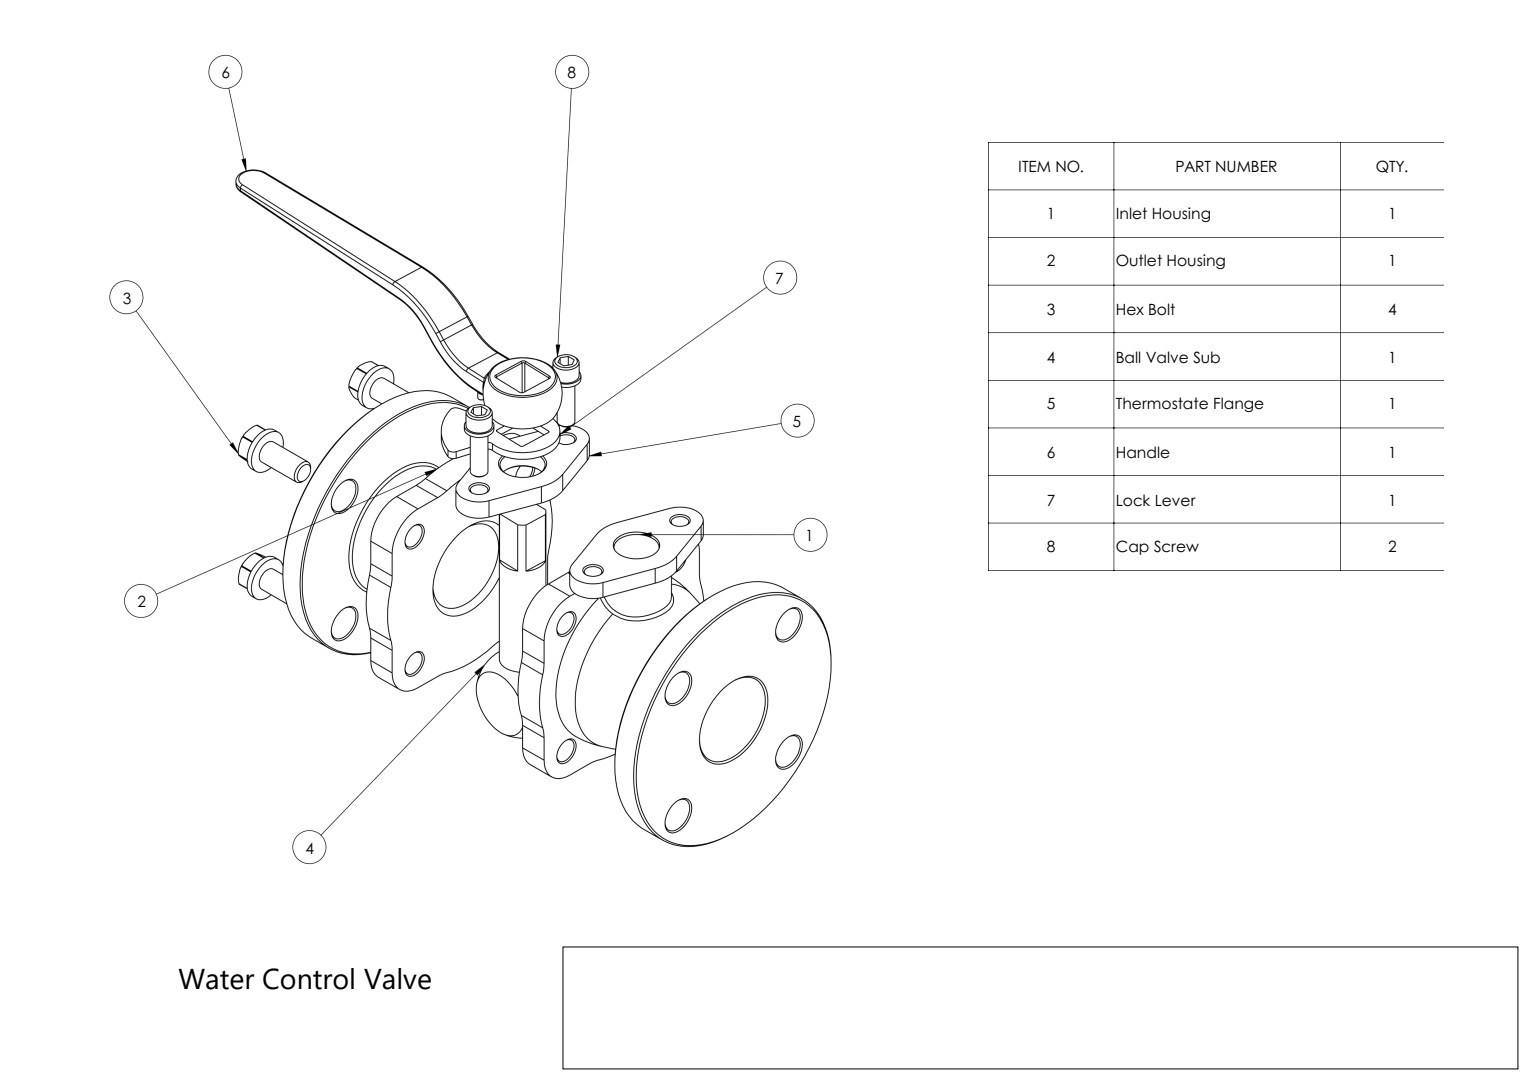
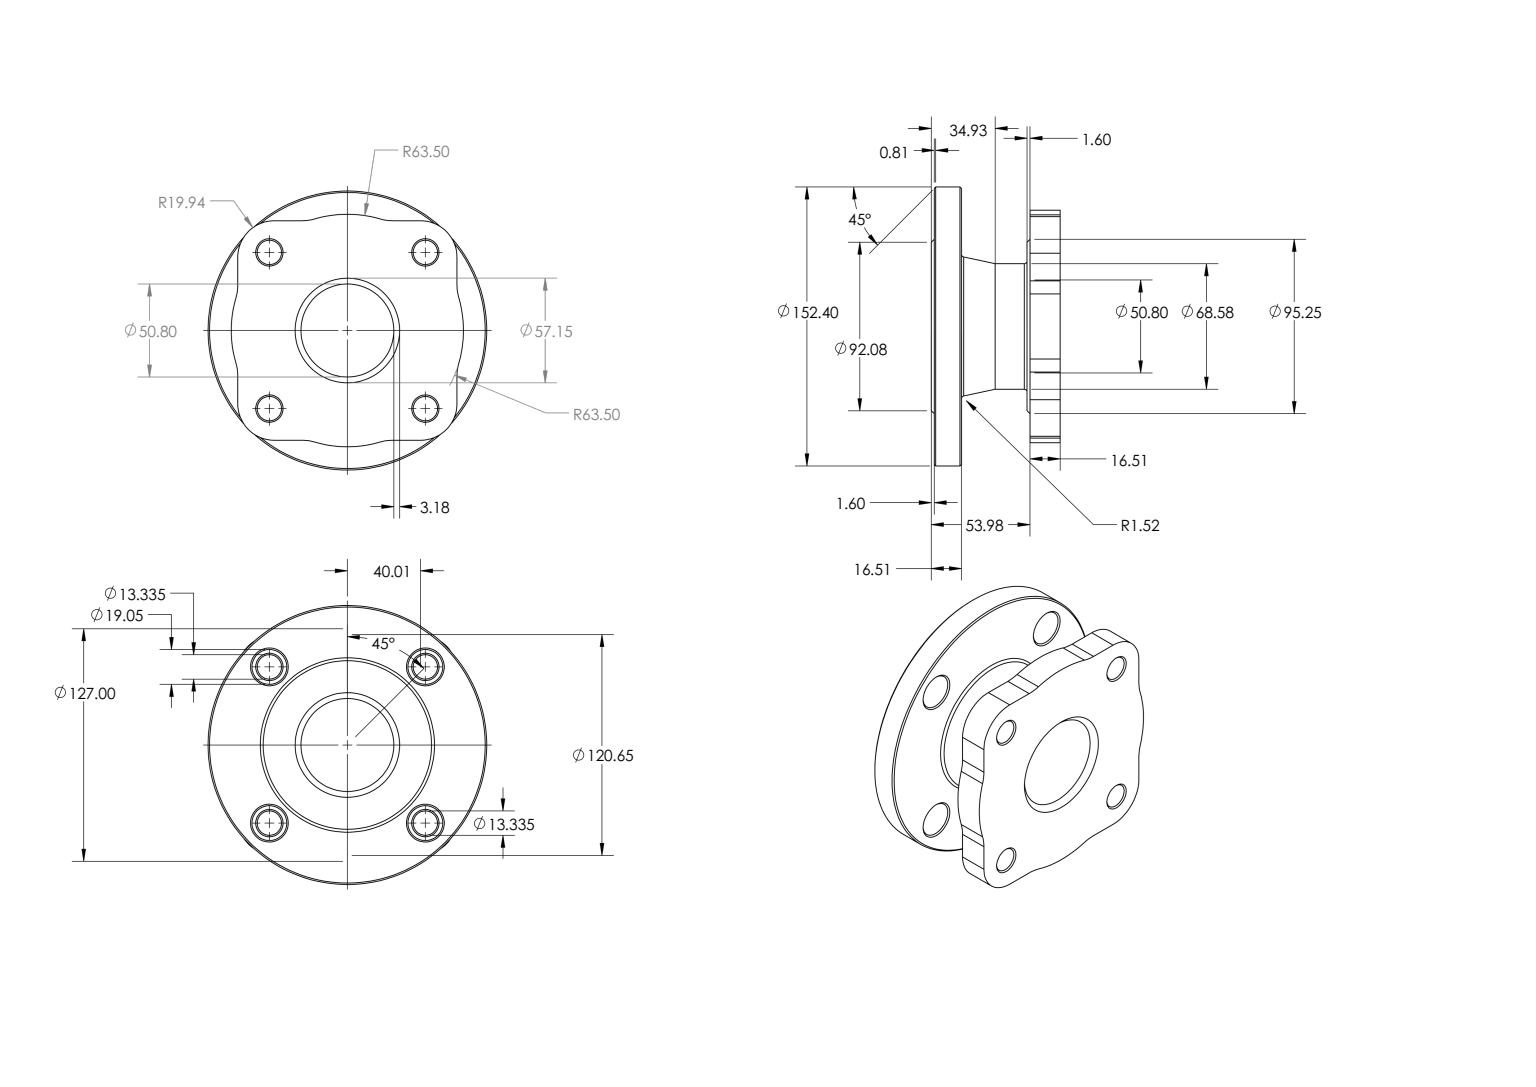
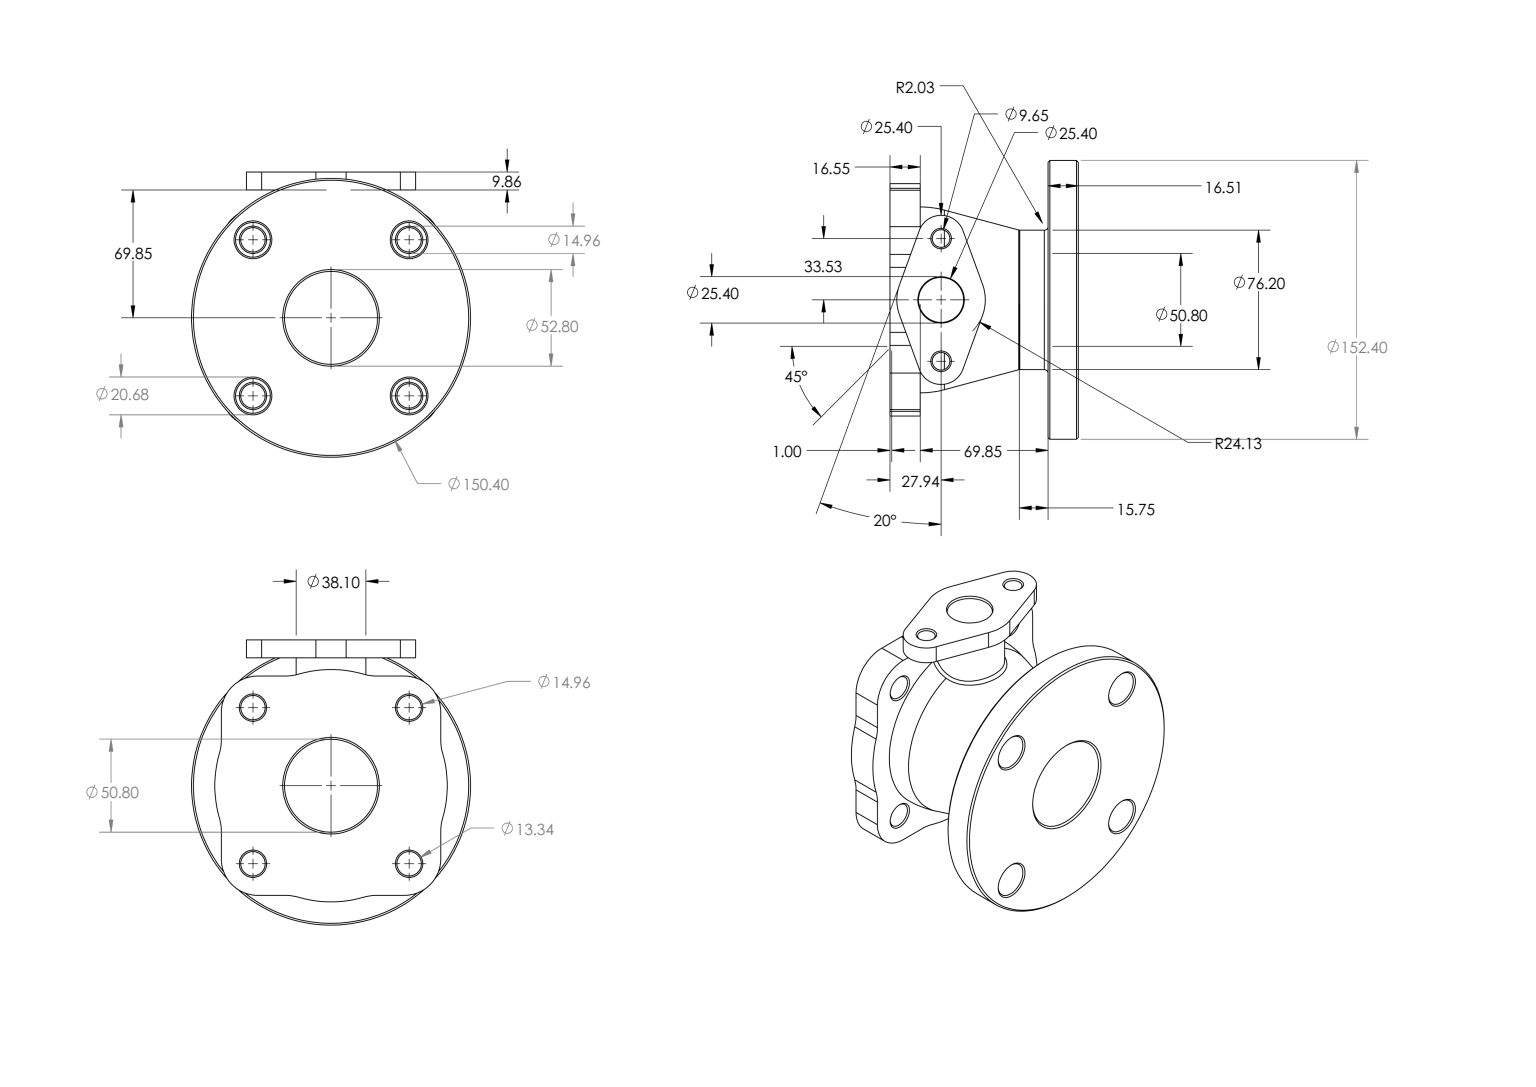
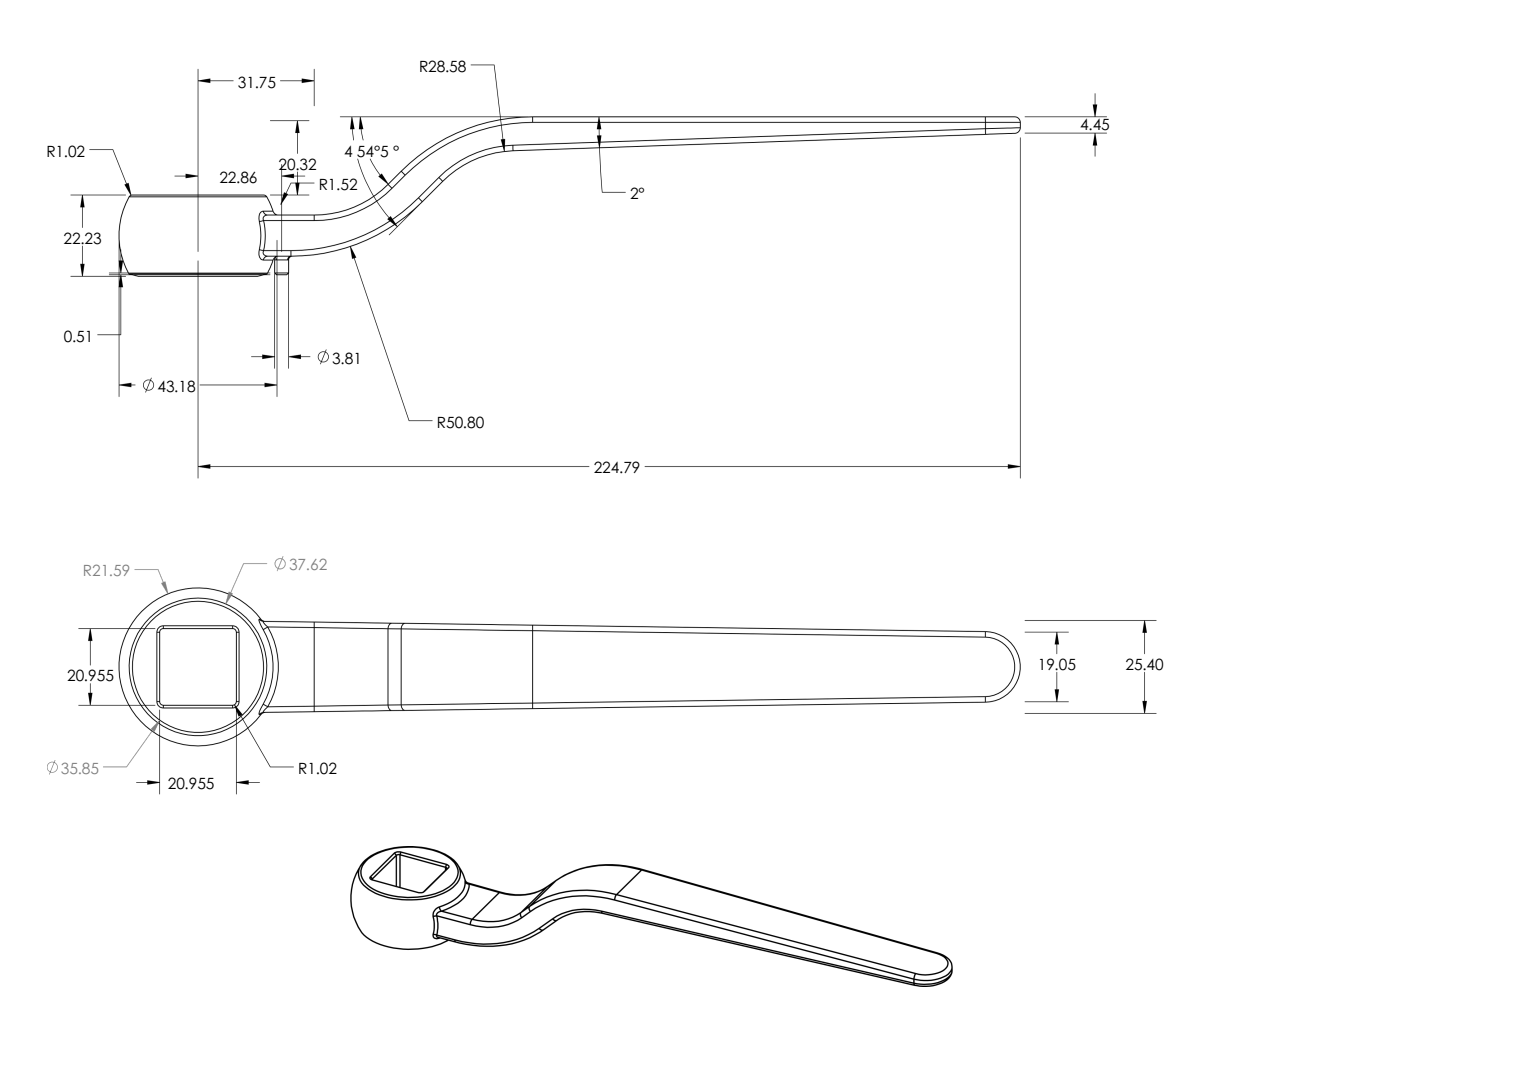
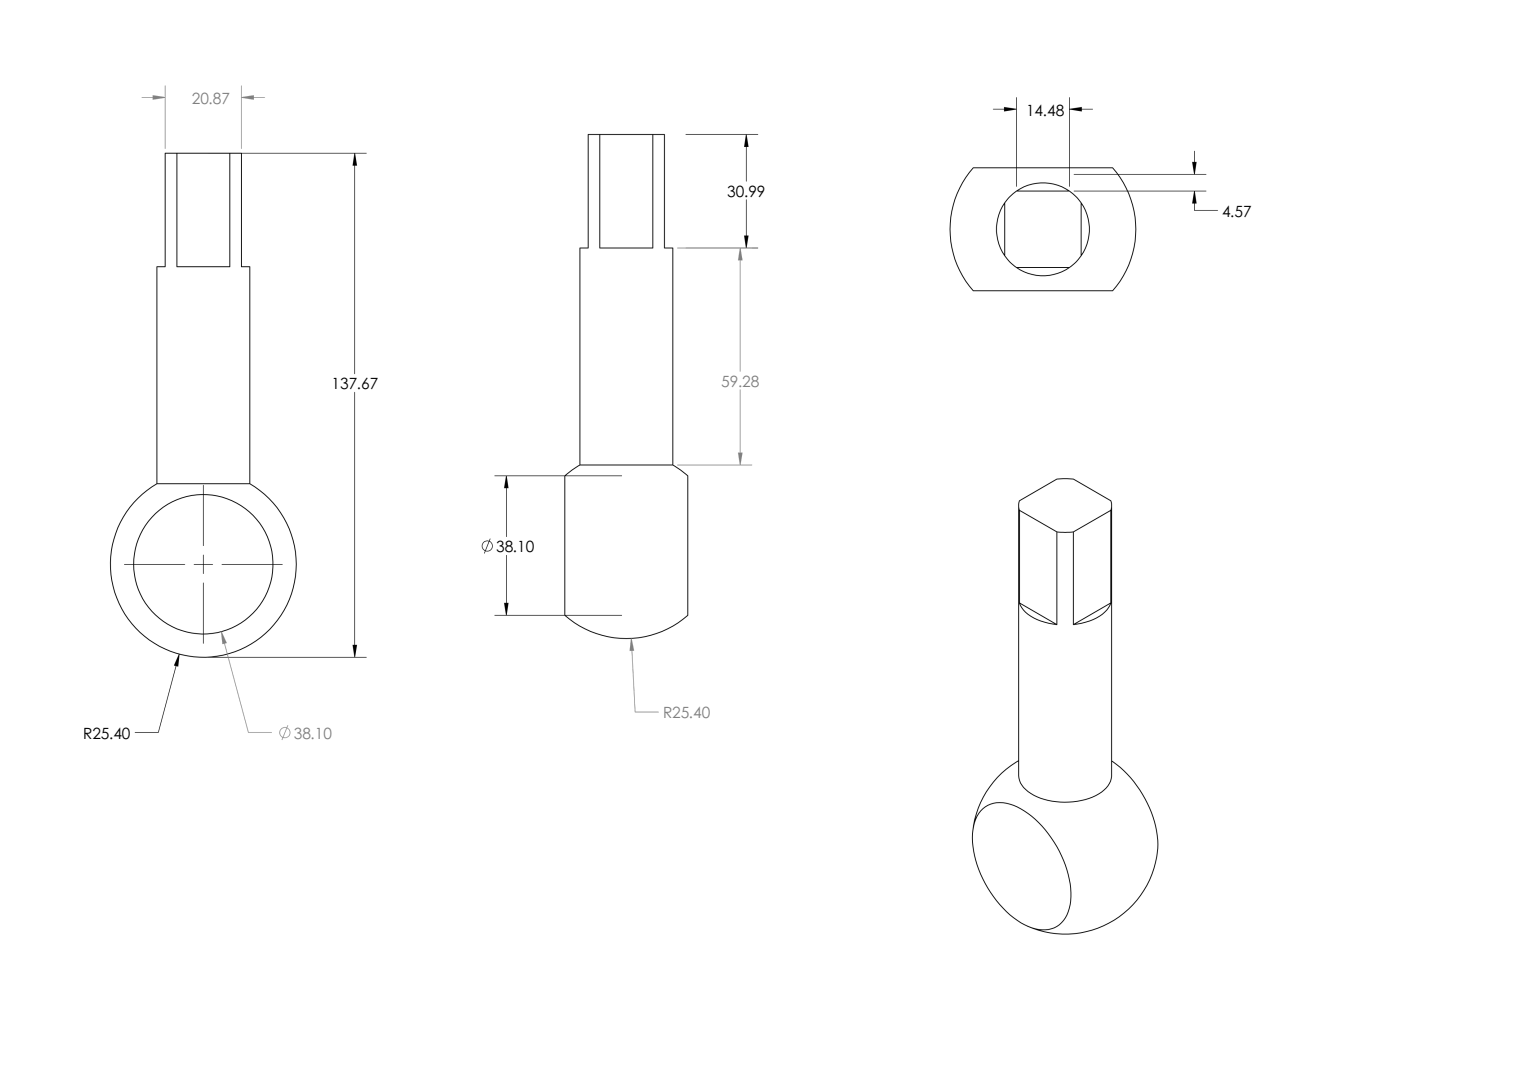
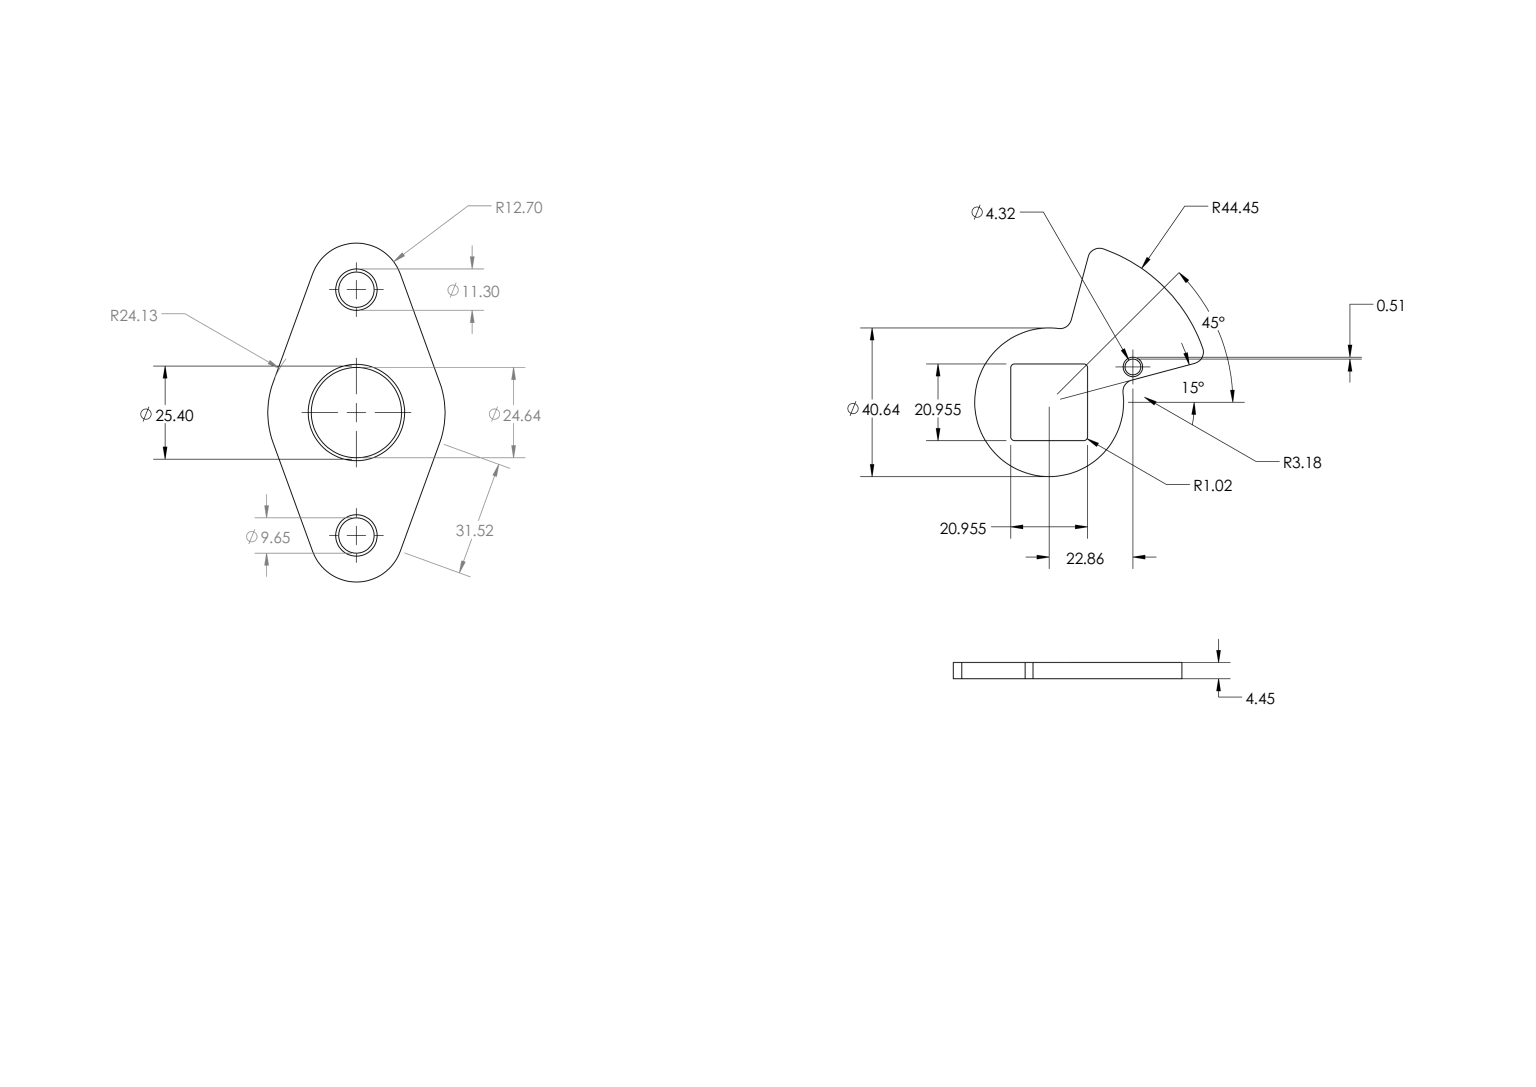
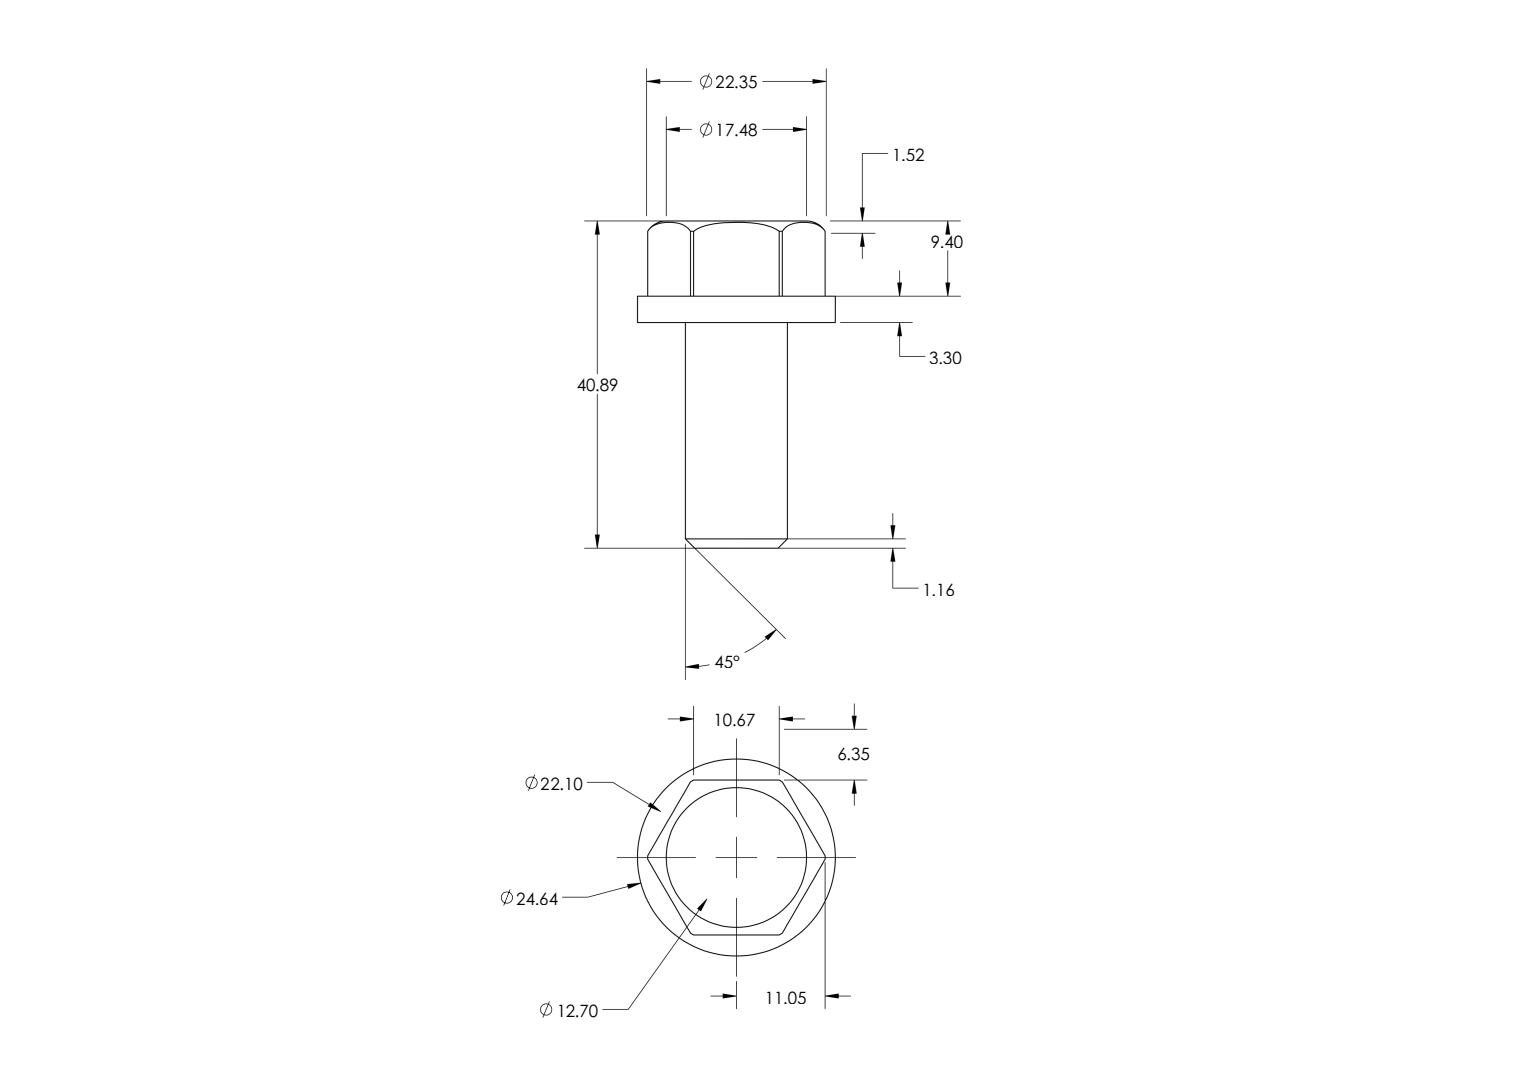
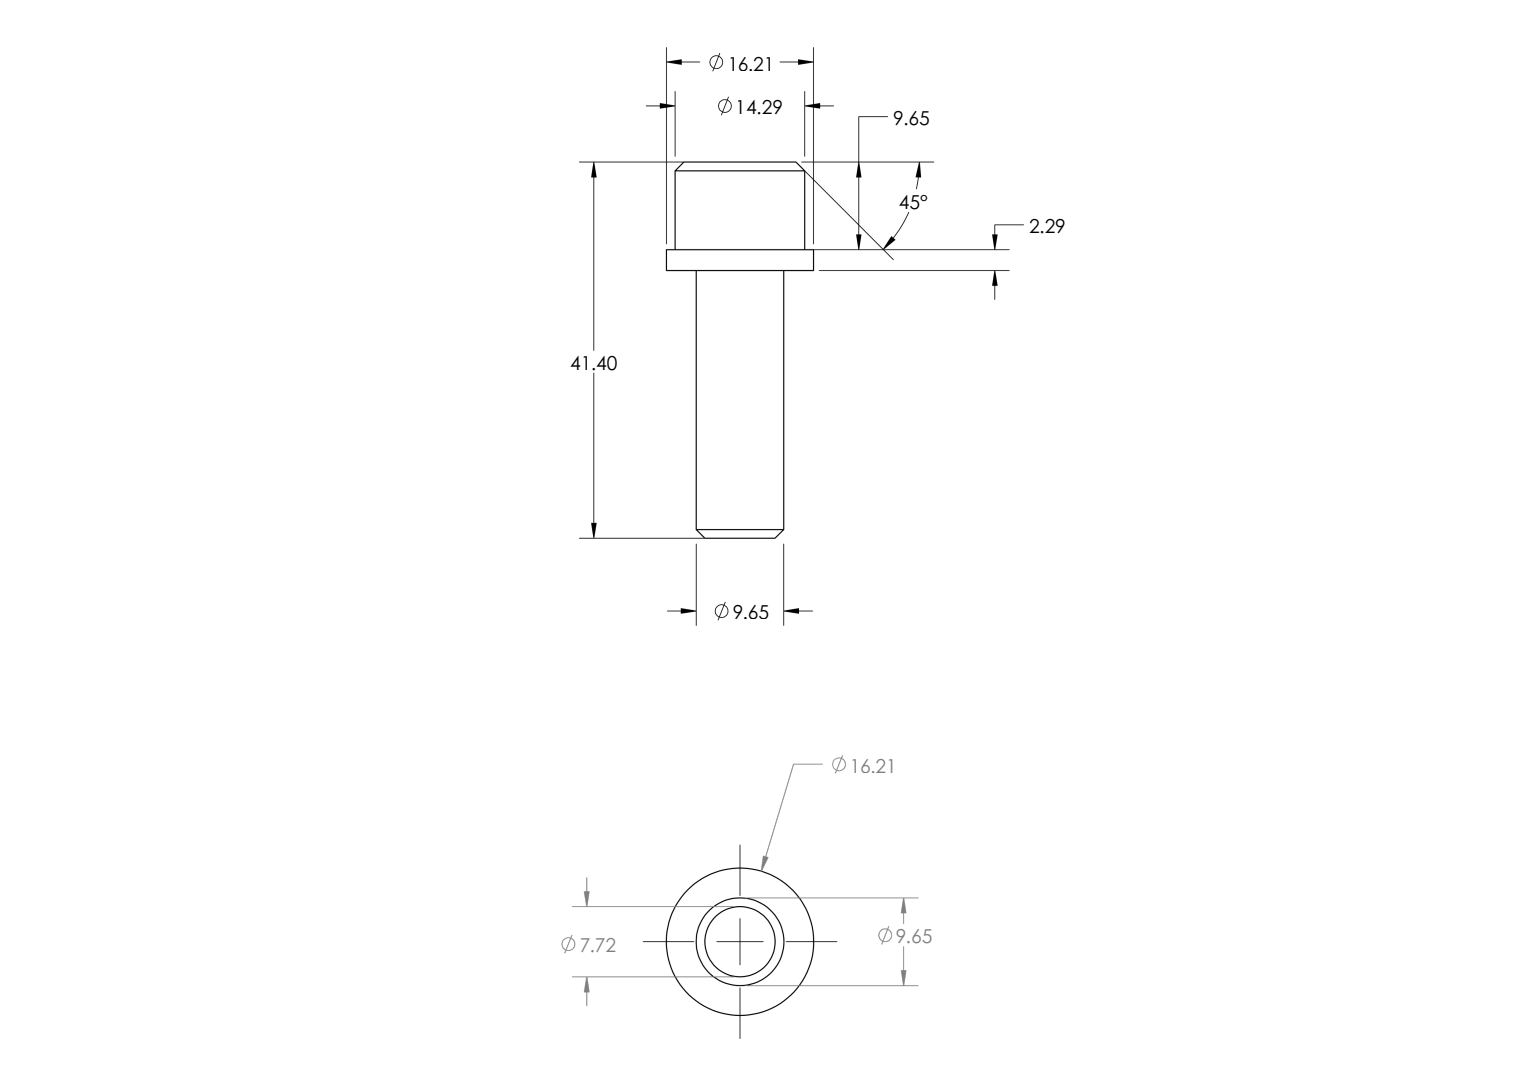
ISO-10303-21;
HEADER;
FILE_DESCRIPTION (('STEP AP214'),
    '1' );
FILE_NAME ('MAT-052',
    '2026-10-23T18:01:19',
    ( '' ),
    ( '' ),
    'SwSTEP 2.0',
    'SolidWorks 2025',
    '' );
FILE_SCHEMA (( 'AUTOMOTIVE_DESIGN' ));
ENDSEC;

DATA;
#1 = ORIENTED_EDGE ( 'NONE', *, *, #12221, .T. ) ;
#2 = CARTESIAN_POINT ( 'NONE',  ( 0.6742552310713171293, -0.4178340986603278351, 0.4797493044159374387 ) ) ;
#3 = CARTESIAN_POINT ( 'NONE',  ( 0.000000000000000000, 0.03800000000000004763, 0.000000000000000000 ) ) ;
#4 = DIRECTION ( 'NONE',  ( 0.000000000000000000, 0.000000000000000000, -1.000000000000000000 ) ) ;
#5 = ORIENTED_EDGE ( 'NONE', *, *, #15122, .F. ) ;
#6 = MECHANICAL_DESIGN_GEOMETRIC_PRESENTATION_REPRESENTATION (  '', ( #7130 ), #10291 ) ;
#7 = CYLINDRICAL_SURFACE ( 'NONE', #13072, 0.7849999999999998090 ) ;
#8 = EDGE_LOOP ( 'NONE', ( #3348, #3892, #6424, #10315, #10248, #3759, #9875, #3838 ) ) ;
#9 = DIRECTION ( 'NONE',  ( 0.000000000000000000, 1.000000000000000000, 0.000000000000000000 ) ) ;
#10 = DIRECTION ( 'NONE',  ( 0.000000000000000000, 0.000000000000000000, 1.000000000000000000 ) ) ;
#11 = ORIENTED_EDGE ( 'NONE', *, *, #1358, .T. ) ;
#12 = CARTESIAN_POINT ( 'NONE',  ( 2.742999999999999883, -1.679378605318041950, 1.679378605318059048 ) ) ;
#13 = ADVANCED_FACE ( 'NONE', ( #4673 ), #12779, .T. ) ;
#14 = CARTESIAN_POINT ( 'NONE',  ( 2.184227569363842658, 0.01449120636726281344, -0.4691493281163300333 ) ) ;
#15 = DIRECTION ( 'NONE',  ( 0.01412288512831213171, -3.675428035873182550E-19, -0.9999002670844991947 ) ) ;
#16 = AXIS2_PLACEMENT_3D ( 'NONE', #9213, #3471, #11656 ) ;
#17 = CARTESIAN_POINT ( 'NONE',  ( 2.124999999999999556, 2.359999999999994547, -1.575000000000016831 ) ) ;
#18 = CARTESIAN_POINT ( 'NONE',  ( 3.512958614626789711, 1.913572711384756708, -0.7285857137282393259 ) ) ;
#19 = ORIENTED_EDGE ( 'NONE', *, *, #5081, .F. ) ;
#20 = EDGE_LOOP ( 'NONE', ( #12977, #13926, #80, #12330, #3550, #1195, #10646, #7919 ) ) ;
#21 = CARTESIAN_POINT ( 'NONE',  ( 1.014389565038390506, -0.4429482523290907969, -0.3623444146133236177 ) ) ;
#22 = EDGE_LOOP ( 'NONE', ( #257, #9527, #1751, #1680 ) ) ;
#23 = AXIS2_PLACEMENT_3D ( 'NONE', #11429, #932, #7837 ) ;
#24 = DIRECTION ( 'NONE',  ( 0.000000000000000000, 0.000000000000000000, -1.000000000000000000 ) ) ;
#25 = CARTESIAN_POINT ( 'NONE',  ( 0.9160226681002169302, -0.4626215099191109403, -0.4483450520235250925 ) ) ;
#26 = CARTESIAN_POINT ( 'NONE',  ( 0.7513246802501661881, 0.000000000000000000, -0.4293820849162031661 ) ) ;
#27 = ORIENTED_EDGE ( 'NONE', *, *, #241, .F. ) ;
#28 = EDGE_CURVE ( 'NONE', #11196, #3954, #11572, .T. ) ;
#29 = CARTESIAN_POINT ( 'NONE',  ( 3.875000000000000000, 1.885381157978844868, -0.5000000000000002220 ) ) ;
#30 = CARTESIAN_POINT ( 'NONE',  ( 2.774999999999999911, -0.9799999999999436939, 2.360000000000016307 ) ) ;
#31 = DIRECTION ( 'NONE',  ( -1.000000000000000000, -0.000000000000000000, -0.000000000000000000 ) ) ;
#32 = CARTESIAN_POINT ( 'NONE',  ( 3.874999999999999556, 3.567999999999999616, -1.320000000000000062 ) ) ;
#33 = CARTESIAN_POINT ( 'NONE',  ( 4.627329080935005834, 1.724141250851881191, -0.2956774535502572077 ) ) ;
#34 = VERTEX_POINT ( 'NONE', #12922 ) ;
#36 = EDGE_LOOP ( 'NONE', ( #14330, #7722, #9947, #11329, #1823, #9061, #6511, #9617 ) ) ;
#35 = CARTESIAN_POINT ( 'NONE',  ( 0.4192535942842503527, 1.577705975193650412, 0.03573697939582392430 ) ) ;
#37 = ORIENTED_EDGE ( 'NONE', *, *, #11617, .T. ) ;
#38 = CARTESIAN_POINT ( 'NONE',  ( 2.774999999999999911, -2.360000000000000320, 0.9799999999999999822 ) ) ;
#39 = VERTEX_POINT ( 'NONE', #10557 ) ;
#40 = ADVANCED_FACE ( 'NONE', ( #12760 ), #3290, .F. ) ;
#41 = VECTOR ( 'NONE', #2622, 39.37007874015748143 ) ;
#42 = EDGE_CURVE ( 'NONE', #4100, #13687, #5470, .T. ) ;
#43 = DIRECTION ( 'NONE',  ( -0.9994005049267692398, -7.584452071732532247E-16, -0.03462124711963855683 ) ) ;
#44 = DIRECTION ( 'NONE',  ( 0.000000000000000000, 0.000000000000000000, -1.000000000000000000 ) ) ;
#45 = ORIENTED_EDGE ( 'NONE', *, *, #8856, .F. ) ;
#46 = EDGE_CURVE ( 'NONE', #11318, #5162, #12173, .T. ) ;
#47 = DIRECTION ( 'NONE',  ( -1.000000000000000000, -0.000000000000000000, -0.000000000000000000 ) ) ;
#48 = CARTESIAN_POINT ( 'NONE',  ( -0.09035531712817639061, 1.379999999999999671, 0.1565000000000000280 ) ) ;
#49 = DIRECTION ( 'NONE',  ( 0.000000000000000000, 0.000000000000000000, -1.000000000000000000 ) ) ;
#50 = DIRECTION ( 'NONE',  ( 0.000000000000000000, 0.000000000000000000, 1.000000000000000000 ) ) ;
#51 = AXIS2_PLACEMENT_3D ( 'NONE', #8937, #9020, #9933 ) ;
#52 = EDGE_CURVE ( 'NONE', #3395, #10754, #14120, .T. ) ;
#53 = CARTESIAN_POINT ( 'NONE',  ( 2.742999999999999883, -1.679378605318041950, 1.941878605318059003 ) ) ;
#54 = VECTOR ( 'NONE', #5461, 39.37007874015748143 ) ;
#55 = DIRECTION ( 'NONE',  ( -1.000000000000000000, -0.000000000000000000, 0.000000000000000000 ) ) ;
#56 = CARTESIAN_POINT ( 'NONE',  ( 1.375000000000000000, 1.653273178848927113E-16, -1.350000000000000089 ) ) ;
#57 = CARTESIAN_POINT ( 'NONE',  ( 0.1007315414569005807, 0.000000000000000000, -0.7936328852534507705 ) ) ;
#58 = ORIENTED_EDGE ( 'NONE', *, *, #5402, .F. ) ;
#59 = AXIS2_PLACEMENT_3D ( 'NONE', #1494, #12413, #11192 ) ;
#60 = CARTESIAN_POINT ( 'NONE',  ( 3.426491571325181340, -1.679378605318059048, -1.679378605318041950 ) ) ;
#62 = ORIENTED_EDGE ( 'NONE', *, *, #9280, .T. ) ;
#61 = PLANE ( 'NONE',  #8465 ) ;
#63 = ORIENTED_EDGE ( 'NONE', *, *, #4346, .F. ) ;
#64 = CARTESIAN_POINT ( 'NONE',  ( 3.601417382415921686, 1.056999999999999718, -0.3891265382754440227 ) ) ;
#65 = DIRECTION ( 'NONE',  ( 0.000000000000000000, 0.000000000000000000, 1.000000000000000000 ) ) ;
#66 = ORIENTED_EDGE ( 'NONE', *, *, #9058, .F. ) ;
#67 = FACE_OUTER_BOUND ( 'NONE', #2223, .T. ) ;
#68 = CARTESIAN_POINT ( 'NONE',  ( 0.6601485485260571995, -0.3723516483516483011, -0.5137583810202324131 ) ) ;
#69 = AXIS2_PLACEMENT_3D ( 'NONE', #6911, #5755, #13762 ) ;
#70 = CARTESIAN_POINT ( 'NONE',  ( 0.9652173913043479159, -0.4829999999999998739, -0.3379636412230419551 ) ) ;
#71 = ADVANCED_FACE ( 'NONE', ( #976 ), #2655, .T. ) ;
#72 = ORIENTED_EDGE ( 'NONE', *, *, #13429, .F. ) ;
#73 = DIRECTION ( 'NONE',  ( 0.000000000000000000, 0.000000000000000000, 1.000000000000000000 ) ) ;
#74 = CARTESIAN_POINT ( 'NONE',  ( 0.6773748815706875925, -0.3764079396444214298, 0.4904325581699060521 ) ) ;
#75 = CARTESIAN_POINT ( 'NONE',  ( 2.774999999999999911, 1.679378605318042395, -1.679378605318058604 ) ) ;
#76 = DIRECTION ( 'NONE',  ( 0.3420201433256623846, 0.000000000000000000, 0.9396926207859106484 ) ) ;
#77 = ORIENTED_EDGE ( 'NONE', *, *, #5878, .F. ) ;
#78 = EDGE_CURVE ( 'NONE', #7551, #8303, #4616, .T. ) ;
#79 = FACE_OUTER_BOUND ( 'NONE', #9861, .T. ) ;
#80 = ORIENTED_EDGE ( 'NONE', *, *, #10085, .T. ) ;
#81 = DIRECTION ( 'NONE',  ( 0.000000000000000000, 0.000000000000000000, -1.000000000000000000 ) ) ;
#82 = ORIENTED_EDGE ( 'NONE', *, *, #11617, .F. ) ;
#83 = AXIS2_PLACEMENT_3D ( 'NONE', #10254, #9341, #11313 ) ;
#84 = DIRECTION ( 'NONE',  ( -0.000000000000000000, -1.000000000000000000, -0.000000000000000000 ) ) ;
#85 = FACE_OUTER_BOUND ( 'NONE', #9329, .T. ) ;
#86 = DIRECTION ( 'NONE',  ( 0.000000000000000000, 0.000000000000000000, 1.000000000000000000 ) ) ;
#87 = DIRECTION ( 'NONE',  ( -1.000000000000000000, -0.000000000000000000, -0.000000000000000000 ) ) ;
#88 = EDGE_CURVE ( 'NONE', #13385, #4765, #4744, .T. ) ;
#89 = EDGE_LOOP ( 'NONE', ( #7077, #10683, #6520, #11153 ) ) ;
#90 = ORIENTED_EDGE ( 'NONE', *, *, #12016, .T. ) ;
#91 = ORIENTED_EDGE ( 'NONE', *, *, #3376, .F. ) ;
#92 = FACE_BOUND ( 'NONE', #13262, .T. ) ;
#93 = DIRECTION ( 'NONE',  ( -0.000000000000000000, -1.000000000000000000, -0.000000000000000000 ) ) ;
#94 = LINE ( 'NONE', #8250, #10804 ) ;
#95 = CARTESIAN_POINT ( 'NONE',  ( 0.000000000000000000, 4.529999999999999361, 0.000000000000000000 ) ) ;
#96 = AXIS2_PLACEMENT_3D ( 'NONE', #10060, #3097, #1937 ) ;
#97 = CARTESIAN_POINT ( 'NONE',  ( 0.7020471549603389816, -0.02897145875702579823, -0.4816513823572634578 ) ) ;
#98 = ORIENTED_EDGE ( 'NONE', *, *, #14017, .F. ) ;
#99 = CARTESIAN_POINT ( 'NONE',  ( 0.4125000000000000333, 0.1749999999999999889, 0.3724999999999999978 ) ) ;
#100 = AXIS2_PLACEMENT_3D ( 'NONE', #9537, #4707, #14178 ) ;
#101 = AXIS2_PLACEMENT_3D ( 'NONE', #4920, #3459, #11799 ) ;
#102 = DIRECTION ( 'NONE',  ( 0.000000000000000000, 1.000000000000000000, -0.000000000000000000 ) ) ;
#103 = CARTESIAN_POINT ( 'NONE',  ( 3.390179639970223313, 0.6913388717410868800, -0.3921396980529558429 ) ) ;
#104 = FACE_OUTER_BOUND ( 'NONE', #11519, .T. ) ;
#105 = VECTOR ( 'NONE', #3673, 39.37007874015748854 ) ;
#106 = CARTESIAN_POINT ( 'NONE',  ( 4.657203315104130326, 1.728603760376735909, 0.2078873897356731115 ) ) ;
#107 = ORIENTED_EDGE ( 'NONE', *, *, #12678, .F. ) ;
#108 = CIRCLE ( 'NONE', #2074, 0.03999999999999998002 ) ;
#110 = ORIENTED_EDGE ( 'NONE', *, *, #10895, .T. ) ;
#109 = DIRECTION ( 'NONE',  ( 0.000000000000000000, 0.000000000000000000, -1.000000000000000000 ) ) ;
#111 = CIRCLE ( 'NONE', #4039, 0.3750000000000004996 ) ;
#112 = ORIENTED_EDGE ( 'NONE', *, *, #14877, .T. ) ;
#113 = CARTESIAN_POINT ( 'NONE',  ( 0.8418300605894719624, -0.4829999999999998739, -0.3276580719765713745 ) ) ;
#114 = VERTEX_POINT ( 'NONE', #12839 ) ;
#115 = CARTESIAN_POINT ( 'NONE',  ( 6.826491571325181695, 0.000000000000000000, 0.000000000000000000 ) ) ;
#116 = APPLICATION_PROTOCOL_DEFINITION ( 'draft international standard', 'automotive_design', 1998, #8901 ) ;
#117 = CARTESIAN_POINT ( 'NONE',  ( 2.774999999999999911, 3.360000000000016751, 0.9799999999999461364 ) ) ;
#118 = ORIENTED_EDGE ( 'NONE', *, *, #160, .F. ) ;
#119 = CARTESIAN_POINT ( 'NONE',  ( -0.09057123220595257596, 1.599173898159329976, -0.3809527529760086129 ) ) ;
#120 = CARTESIAN_POINT ( 'NONE',  ( 2.061999999999999389, 0.000000000000000000, 0.000000000000000000 ) ) ;
#121 = CIRCLE ( 'NONE', #850, 0.1899999999999996136 ) ;
#122 = CARTESIAN_POINT ( 'NONE',  ( 3.874999999999999556, 2.750000000000000000, -1.320000000000000062 ) ) ;
#123 = CIRCLE ( 'NONE', #13312, 0.2944999999999987073 ) ;
#124 = CIRCLE ( 'NONE', #8691, 0.9999999999999996669 ) ;
#125 = ADVANCED_FACE ( 'NONE', ( #8119 ), #11202, .T. ) ;
#126 = DIRECTION ( 'NONE',  ( 0.000000000000000000, 0.000000000000000000, 1.000000000000000000 ) ) ;
#127 = CARTESIAN_POINT ( 'NONE',  ( 2.124999999999999556, -0.6999999999999598765, 2.400000000000012346 ) ) ;
#128 = DIRECTION ( 'NONE',  ( 0.7071067811865459074, -0.7071067811865492381, 0.000000000000000000 ) ) ;
#129 = AXIS2_PLACEMENT_3D ( 'NONE', #12929, #1218, #11933 ) ;
#130 = ORIENTED_EDGE ( 'NONE', *, *, #6487, .T. ) ;
#131 = CARTESIAN_POINT ( 'NONE',  ( 2.774999999999999911, 2.360000000000015863, 1.574999999999999956 ) ) ;
#133 = EDGE_LOOP ( 'NONE', ( #9480, #11934, #9524, #6761 ) ) ;
#132 = CARTESIAN_POINT ( 'NONE',  ( 0.000000000000000000, 0.000000000000000000, 0.000000000000000000 ) ) ;
#134 = ORIENTED_EDGE ( 'NONE', *, *, #1959, .F. ) ;
#135 = CIRCLE ( 'NONE', #14993, 0.7849999999999993650 ) ;
#136 = FACE_OUTER_BOUND ( 'NONE', #12337, .T. ) ;
#137 = ADVANCED_FACE ( 'NONE', ( #6971 ), #13149, .T. ) ;
#138 = CARTESIAN_POINT ( 'NONE',  ( 0.2849999999999996425, 0.000000000000000000, 0.4108223460329292753 ) ) ;
#139 = LINE ( 'NONE', #8292, #12561 ) ;
#140 = EDGE_LOOP ( 'NONE', ( #8999, #12949, #3584, #329, #10455, #10394, #1093, #10887, #312, #1729, #3941 ) ) ;
#141 = CARTESIAN_POINT ( 'NONE',  ( 2.124999999999999556, -1.679378605318041950, 1.973878605318058810 ) ) ;
#142 = CIRCLE ( 'NONE', #9202, 0.3750000000000007772 ) ;
#143 = PLANE ( 'NONE',  #5754 ) ;
#144 = EDGE_CURVE ( 'NONE', #5162, #1223, #2289, .T. ) ;
#145 = CARTESIAN_POINT ( 'NONE',  ( 6.123233995736763571E-17, 4.529999999999999361, 0.4999999999999997224 ) ) ;
#146 = ORIENTED_EDGE ( 'NONE', *, *, #13885, .T. ) ;
#147 = EDGE_CURVE ( 'NONE', #7267, #14527, #433, .T. ) ;
#148 = CARTESIAN_POINT ( 'NONE',  ( 0.6894183887957248125, -0.4431162156558585696, 0.4464953827605262493 ) ) ;
#149 = CONICAL_SURFACE ( 'NONE', #9948, 0.2944999999999987073, 0.7853981633974366217 ) ;
#150 = CARTESIAN_POINT ( 'NONE',  ( 3.875000000000000000, 3.137999999999999901, 0.5000000000000002220 ) ) ;
#151 = DIRECTION ( 'NONE',  ( -1.000000000000000000, -0.000000000000000000, -0.000000000000000000 ) ) ;
#152 = EDGE_LOOP ( 'NONE', ( #2875, #13382, #6419, #11719 ) ) ;
#153 = CYLINDRICAL_SURFACE ( 'NONE', #7144, 1.000000000000000444 ) ;
#154 = CARTESIAN_POINT ( 'NONE',  ( -0.4349147617188414694, 0.7512260236060024354, -0.008611041693271251005 ) ) ;
#155 = ORIENTED_EDGE ( 'NONE', *, *, #13397, .T. ) ;
#156 = EDGE_CURVE ( 'NONE', #504, #12467, #11937, .T. ) ;
#157 = CIRCLE ( 'NONE', #12372, 0.05999999999999990757 ) ;
#158 = DIRECTION ( 'NONE',  ( 1.000000000000000000, 0.000000000000000000, 0.000000000000000000 ) ) ;
#159 = VERTEX_POINT ( 'NONE', #11630 ) ;
#160 = EDGE_CURVE ( 'NONE', #1104, #11415, #8533, .T. ) ;
#161 = CARTESIAN_POINT ( 'NONE',  ( 3.426491571325181340, -1.679378605318041950, 1.384878605318060174 ) ) ;
#162 = FACE_OUTER_BOUND ( 'NONE', #5866, .T. ) ;
#163 = TOROIDAL_SURFACE ( 'NONE', #642, 0.3203340137431718859, 0.05999999999999999778 ) ;
#164 = CARTESIAN_POINT ( 'NONE',  ( -0.3724999999999999423, 0.1749999999999999889, 0.3724999999999999978 ) ) ;
#165 = CARTESIAN_POINT ( 'NONE',  ( 3.874999999999999556, 3.567999999999999616, -1.320000000000000062 ) ) ;
#166 = ORIENTED_EDGE ( 'NONE', *, *, #13997, .F. ) ;
#167 = VERTEX_POINT ( 'NONE', #2214 ) ;
#168 = DIRECTION ( 'NONE',  ( 1.000000000000000000, 0.000000000000000000, 0.000000000000000000 ) ) ;
#169 = AXIS2_PLACEMENT_3D ( 'NONE', #3610, #8290, #3527 ) ;
#170 = EDGE_LOOP ( 'NONE', ( #1546, #1638, #4736, #4813 ) ) ;
#171 = EDGE_CURVE ( 'NONE', #13385, #5675, #9017, .T. ) ;
#172 = DIRECTION ( 'NONE',  ( 1.000000000000000000, 0.000000000000000000, 0.000000000000000000 ) ) ;
#173 = CARTESIAN_POINT ( 'NONE',  ( -0.3725000000000000533, -0.6590000000000000302, 0.3724999999999999423 ) ) ;
#174 = EDGE_CURVE ( 'NONE', #282, #4996, #14362, .T. ) ;
#175 = CARTESIAN_POINT ( 'NONE',  ( 0.8848438321385330152, -0.4627371489994540066, -0.4487466038575088079 ) ) ;
#176 = DIRECTION ( 'NONE',  ( 0.01412288512831128343, 0.000000000000000000, 0.9999002670844990837 ) ) ;
#177 = ORIENTED_EDGE ( 'NONE', *, *, #5280, .F. ) ;
#178 = CARTESIAN_POINT ( 'NONE',  ( 3.652559170054249904, 1.936257245559476869, -0.4479448007622380823 ) ) ;
#179 = CONICAL_SURFACE ( 'NONE', #7293, 0.5174999999999995159, 0.7853981633974514986 ) ;
#180 = ADVANCED_FACE ( 'NONE', ( #3680 ), #7071, .F. ) ;
#181 = CARTESIAN_POINT ( 'NONE',  ( 1.397260334976607732, 0.007251848866960360247, 0.4201477693899102750 ) ) ;
#182 = DIRECTION ( 'NONE',  ( 0.000000000000000000, 0.000000000000000000, -1.000000000000000000 ) ) ;
#183 = VECTOR ( 'NONE', #7595, 39.37007874015748143 ) ;
#184 = VERTEX_POINT ( 'NONE', #11856 ) ;
#186 = EDGE_LOOP ( 'NONE', ( #11801, #8509, #1158, #8869 ) ) ;
#185 = CARTESIAN_POINT ( 'NONE',  ( 2.774999999999999911, 0.000000000000000000, 0.000000000000000000 ) ) ;
#187 = ORIENTED_EDGE ( 'NONE', *, *, #8888, .T. ) ;
#188 = DIRECTION ( 'NONE',  ( 1.000000000000000000, 0.000000000000000000, 0.000000000000000000 ) ) ;
#189 = ORIENTED_EDGE ( 'NONE', *, *, #6062, .T. ) ;
#190 = CARTESIAN_POINT ( 'NONE',  ( 3.426491571325181340, 0.000000000000000000, 0.000000000000000000 ) ) ;
#191 = ITEM_DEFINED_TRANSFORMATION ( 'NONE', 'NONE', #14264,  #8424 ) ;
#192 = FACE_BOUND ( 'NONE', #6135, .T. ) ;
#193 = VERTEX_POINT ( 'NONE', #1581 ) ;
#194 = CIRCLE ( 'NONE', #13862, 0.4349999999999999978 ) ;
#195 = CARTESIAN_POINT ( 'NONE',  ( -0.1702285915635917690, 1.581112972951822293, -0.3809527529760087239 ) ) ;
#196 = PLANE ( 'NONE',  #6331 ) ;
#197 = AXIS2_PLACEMENT_3D ( 'NONE', #7203, #5970, #10632 ) ;
#198 = EDGE_CURVE ( 'NONE', #9755, #1223, #6326, .T. ) ;
#199 = FACE_OUTER_BOUND ( 'NONE', #10241, .T. ) ;
#200 = DIRECTION ( 'NONE',  ( -1.000000000000000000, 0.000000000000000000, -1.047444401652940007E-14 ) ) ;
#201 = AXIS2_PLACEMENT_3D ( 'NONE', #268, #9637, #13052 ) ;
#202 = AXIS2_PLACEMENT_3D ( 'NONE', #13035, #253, #10606 ) ;
#203 = PLANE ( 'NONE',  #5048 ) ;
#204 = CARTESIAN_POINT ( 'NONE',  ( 0.4193347797797013499, 0.1749999999999999889, -1.564978703518711711 ) ) ;
#205 = LINE ( 'NONE', #13137, #4871 ) ;
#206 = CARTESIAN_POINT ( 'NONE',  ( 4.545987629778766248, 1.714706108888804481, 0.4425078797212881887 ) ) ;
#207 = ORIENTED_EDGE ( 'NONE', *, *, #6693, .F. ) ;
#208 = AXIS2_PLACEMENT_3D ( 'NONE', #5410, #13799, #3334 ) ;
#209 = DIRECTION ( 'NONE',  ( 0.000000000000000000, 0.000000000000000000, 1.000000000000000000 ) ) ;
#211 = ORIENTED_EDGE ( 'NONE', *, *, #10111, .F. ) ;
#210 = DIRECTION ( 'NONE',  ( -1.000000000000000000, -0.000000000000000000, -0.000000000000000000 ) ) ;
#212 = ORIENTED_EDGE ( 'NONE', *, *, #11674, .T. ) ;
#213 = VECTOR ( 'NONE', #1409, 39.37007874015748143 ) ;
#214 = FACE_OUTER_BOUND ( 'NONE', #11433, .T. ) ;
#215 = LENGTH_MEASURE_WITH_UNIT ( LENGTH_MEASURE( 0.02539999999999999897 ), #6283 );
#216 = DIRECTION ( 'NONE',  ( 1.000000000000000000, 0.000000000000000000, 0.000000000000000000 ) ) ;
#217 = ORIENTED_EDGE ( 'NONE', *, *, #5293, .F. ) ;
#218 = CARTESIAN_POINT ( 'NONE',  ( 6.787121492585022509, 0.000000000000000000, 0.000000000000000000 ) ) ;
#219 = ADVANCED_FACE ( 'NONE', ( #3751 ), #1356, .F. ) ;
#220 = CARTESIAN_POINT ( 'NONE',  ( 3.601417382415921686, 1.056999999999999718, 0.5000000000000000000 ) ) ;
#221 = DIRECTION ( 'NONE',  ( 0.01412288512831213171, -3.675428035873182550E-19, 0.9999002670844991947 ) ) ;
#222 = AXIS2_PLACEMENT_3D ( 'NONE', #2084, #6691, #5471 ) ;
#223 = ORIENTED_EDGE ( 'NONE', *, *, #6094, .T. ) ;
#224 = CARTESIAN_POINT ( 'NONE',  ( 0.4425000000000003375, 0.2159999999999999420, 0.3724999999999999423 ) ) ;
#225 = LINE ( 'NONE', #9876, #6827 ) ;
#226 = PLANE ( 'NONE',  #3739 ) ;
#227 = CARTESIAN_POINT ( 'NONE',  ( 0.7936328852534488831, 0.1749999999999999889, -0.1007315414569159018 ) ) ;
#228 = ORIENTED_EDGE ( 'NONE', *, *, #3551, .T. ) ;
#229 = DIRECTION ( 'NONE',  ( 0.7071067811865474617, 8.659560562354932858E-17, 0.7071067811865474617 ) ) ;
#230 = ORIENTED_EDGE ( 'NONE', *, *, #13541, .F. ) ;
#231 = CARTESIAN_POINT ( 'NONE',  ( -0.2846118995245673911, 1.599166939805956256, 0.2689432355367775695 ) ) ;
#232 = ORIENTED_EDGE ( 'NONE', *, *, #13602, .F. ) ;
#233 = EDGE_CURVE ( 'NONE', #5394, #8971, #13378, .T. ) ;
#234 = CARTESIAN_POINT ( 'NONE',  ( 3.874999999999999556, 3.567999999999999616, -1.130000000000000560 ) ) ;
#235 = EDGE_CURVE ( 'NONE', #5730, #4833, #8634, .T. ) ;
#236 = EDGE_CURVE ( 'NONE', #4318, #1348, #8143, .T. ) ;
#237 = LINE ( 'NONE', #14244, #10985 ) ;
#238 = CARTESIAN_POINT ( 'NONE',  ( 1.000847373107697891, -0.4430000000000000049, 0.4858637376679703634 ) ) ;
#239 = FACE_OUTER_BOUND ( 'NONE', #14821, .T. ) ;
#240 = DIRECTION ( 'NONE',  ( -0.000000000000000000, 1.000000000000000000, -0.000000000000000000 ) ) ;
#241 = EDGE_CURVE ( 'NONE', #287, #6694, #6272, .T. ) ;
#242 = LINE ( 'NONE', #7239, #4272 ) ;
#243 = AXIS2_PLACEMENT_3D ( 'NONE', #9319, #1107, #15044 ) ;
#244 = ORIENTED_EDGE ( 'NONE', *, *, #5155, .F. ) ;
#245 = ORIENTED_EDGE ( 'NONE', *, *, #2104, .F. ) ;
#246 = ORIENTED_EDGE ( 'NONE', *, *, #3419, .T. ) ;
#247 = CARTESIAN_POINT ( 'NONE',  ( 1.012992808803494293, -0.4429593110677563228, -0.3529645107950314387 ) ) ;
#248 = FACE_OUTER_BOUND ( 'NONE', #14126, .T. ) ;
#249 = CARTESIAN_POINT ( 'NONE',  ( 3.602264755523620465, 0.9969999999999996643, 0.4491205543005138412 ) ) ;
#250 = DIRECTION ( 'NONE',  ( 0.000000000000000000, 1.000000000000000000, -0.000000000000000000 ) ) ;
#251 = VERTEX_POINT ( 'NONE', #2745 ) ;
#252 = DIRECTION ( 'NONE',  ( -1.150251786806006500E-15, 0.000000000000000000, 1.000000000000000000 ) ) ;
#253 = DIRECTION ( 'NONE',  ( 1.365923996832131609E-16, -1.000000000000000000, -0.000000000000000000 ) ) ;
#254 = CYLINDRICAL_SURFACE ( 'NONE', #1961, 2.500000000000000444 ) ;
#255 = EDGE_CURVE ( 'NONE', #14724, #7714, #12509, .T. ) ;
#256 = CIRCLE ( 'NONE', #12476, 0.4999999999999995004 ) ;
#257 = ORIENTED_EDGE ( 'NONE', *, *, #5350, .T. ) ;
#259 = VERTEX_POINT ( 'NONE', #10708 ) ;
#258 = DIRECTION ( 'NONE',  ( -1.000000000000000000, -0.000000000000000000, -0.000000000000000000 ) ) ;
#260 = EDGE_CURVE ( 'NONE', #10245, #11406, #12148, .T. ) ;
#261 = VERTEX_POINT ( 'NONE', #9572 ) ;
#262 = CARTESIAN_POINT ( 'NONE',  ( 0.7058998964907862161, -0.05999999999999994227, -0.4900296624789436950 ) ) ;
#263 = ORIENTED_EDGE ( 'NONE', *, *, #11976, .T. ) ;
#264 = APPLICATION_PROTOCOL_DEFINITION ( 'draft international standard', 'automotive_design', 1998, #1849 ) ;
#265 = CARTESIAN_POINT ( 'NONE',  ( 0.6601485485260571995, -0.07064835164835162051, 0.5137583810202324131 ) ) ;
#266 = ORIENTED_EDGE ( 'NONE', *, *, #8038, .T. ) ;
#267 = DIRECTION ( 'NONE',  ( 0.000000000000000000, 0.000000000000000000, -1.000000000000000000 ) ) ;
#268 = CARTESIAN_POINT ( 'NONE',  ( 6.826491571325181695, 1.679378605318059492, 1.679378605318041506 ) ) ;
#269 = CARTESIAN_POINT ( 'NONE',  ( 2.807000000000000828, 1.679378605318042395, -1.679378605318058604 ) ) ;
#270 = TOROIDAL_SURFACE ( 'NONE', #12014, 0.5849999999999996314, 0.1000000000000000056 ) ;
#271 = PRODUCT_DEFINITION_SHAPE ( 'NONE', 'NONE',  #3615 ) ;
#272 = DIRECTION ( 'NONE',  ( -0.000000000000000000, -1.000000000000000000, -0.000000000000000000 ) ) ;
#273 = CARTESIAN_POINT ( 'NONE',  ( 0.8490493353346898475, -0.4471313898566136036, -0.4310079353635160593 ) ) ;
#274 = DIRECTION ( 'NONE',  ( -1.000000000000000000, -0.000000000000000000, -0.000000000000000000 ) ) ;
#275 = CARTESIAN_POINT ( 'NONE',  ( 3.598246013678398914, 1.876591252814830524, 0.7602127166807192138 ) ) ;
#276 = DIRECTION ( 'NONE',  ( -0.9743309173630050335, 0.2251205531944274196, 1.138269997360108984E-15 ) ) ;
#277 = EDGE_CURVE ( 'NONE', #13668, #9005, #9364, .T. ) ;
#278 = ADVANCED_FACE ( 'NONE', ( #14215 ), #6778, .F. ) ;
#279 = ORIENTED_EDGE ( 'NONE', *, *, #7763, .F. ) ;
#280 = CARTESIAN_POINT ( 'NONE',  ( 0.000000000000000000, 1.629999999999999893, 0.000000000000000000 ) ) ;
#282 = VERTEX_POINT ( 'NONE', #8788 ) ;
#281 = DIRECTION ( 'NONE',  ( -0.9396926207859105373, 0.000000000000000000, 0.3420201433256627732 ) ) ;
#283 = ORIENTED_EDGE ( 'NONE', *, *, #1026, .F. ) ;
#284 = CARTESIAN_POINT ( 'NONE',  ( 0.8999999999999999112, -0.6230000000000016636, -0.3750000000000000555 ) ) ;
#285 =( NAMED_UNIT ( * ) PLANE_ANGLE_UNIT ( ) SI_UNIT ( $, .RADIAN. ) );
#286 = CARTESIAN_POINT ( 'NONE',  ( 3.250637184708970562, 0.6799532182389177448, 0.4540870454136761714 ) ) ;
#287 = VERTEX_POINT ( 'NONE', #11147 ) ;
#288 = LINE ( 'NONE', #2465, #664 ) ;
#289 = VECTOR ( 'NONE', #12464, 39.37007874015748854 ) ;
#290 = CARTESIAN_POINT ( 'NONE',  ( 0.7206835787589852549, -0.006955211921962108426, 0.4581197915133168319 ) ) ;
#291 = DIRECTION ( 'NONE',  ( -0.7071067811865600072, -0.7071067811865350272, 1.170732267570241832E-16 ) ) ;
#292 = ORIENTED_EDGE ( 'NONE', *, *, #11564, .F. ) ;
#293 = CARTESIAN_POINT ( 'NONE',  ( 6.826491571325181695, 1.679378605318059492, 1.272378605318041478 ) ) ;
#294 = DIRECTION ( 'NONE',  ( 0.000000000000000000, 0.000000000000000000, 1.000000000000000000 ) ) ;
#295 = CARTESIAN_POINT ( 'NONE',  ( 6.208491571325183145, -1.679378605318047946, -1.679378605318053497 ) ) ;
#296 = ORIENTED_EDGE ( 'NONE', *, *, #3192, .T. ) ;
#297 = CARTESIAN_POINT ( 'NONE',  ( 7.623651669702752511E-17, -0.6589999999999998082, 0.000000000000000000 ) ) ;
#298 = EDGE_LOOP ( 'NONE', ( #11252, #3224, #10809, #13371 ) ) ;
#299 = DIRECTION ( 'NONE',  ( -1.000000000000000000, -0.000000000000000000, 0.000000000000000000 ) ) ;
#300 = ORIENTED_EDGE ( 'NONE', *, *, #13461, .F. ) ;
#301 = FACE_OUTER_BOUND ( 'NONE', #6779, .T. ) ;
#302 = AXIS2_PLACEMENT_3D ( 'NONE', #1388, #8381, #4776 ) ;
#303 = CARTESIAN_POINT ( 'NONE',  ( 6.176491571325181340, 1.679378605318035733, -1.272378605318063016 ) ) ;
#304 = CLOSED_SHELL ( 'NONE', ( #4084, #3715, #13988, #9132, #6250, #7556, #10908, #15018, #4095, #10366, #6449, #8320, #10443, #8270, #3227, #14480, #7146, #10275, #8252, #180, #13730, #1548, #4494, #4329, #612, #13021, #6644, #5400, #14500, #1485, #9870, #4669, #3904, #13, #9470, #71, #4566, #10359, #7820, #13323, #1048, #3821, #137, #7710, #15088, #14323, #12052, #4366, #10484, #5633, #10963, #9242, #8977, #13823, #11177, #7331, #10823, #2508, #13713, #11143, #800, #2244, #6928, #3658, #8862, #8822, #2431, #3980, #11791, #7372, #3340, #12971, #6898, #2775, #778, #5612, #40, #13581, #10360, #10036, #563, #14744, #6065, #10269, #13177, #5255, #5880, #11038, #7201, #6281, #3783, #8051, #13140, #7484, #13786, #10726, #4147, #125, #2428, #3088, #11874, #9994, #9436 ) ) ;
#305 = LINE ( 'NONE', #5012, #4613 ) ;
#306 = CARTESIAN_POINT ( 'NONE',  ( 6.826491571325181695, -1.679378605318048390, 1.272378605318051914 ) ) ;
#307 = EDGE_CURVE ( 'NONE', #9198, #11593, #9851, .T. ) ;
#308 = EDGE_CURVE ( 'NONE', #4201, #2516, #10088, .T. ) ;
#309 = VECTOR ( 'NONE', #6967, 39.37007874015748143 ) ;
#310 = ORIENTED_EDGE ( 'NONE', *, *, #14681, .T. ) ;
#311 = ORIENTED_EDGE ( 'NONE', *, *, #2045, .F. ) ;
#312 = ORIENTED_EDGE ( 'NONE', *, *, #6259, .T. ) ;
#313 = CYLINDRICAL_SURFACE ( 'NONE', #4057, 0.03999999999999998002 ) ;
#314 = DIRECTION ( 'NONE',  ( 0.000000000000000000, 0.000000000000000000, -1.000000000000000000 ) ) ;
#315 = CARTESIAN_POINT ( 'NONE',  ( 0.4108223460329304411, 5.750000000000000000, -0.2849999999999985323 ) ) ;
#316 = ADVANCED_FACE ( 'NONE', ( #874 ), #6177, .F. ) ;
#317 = DIRECTION ( 'NONE',  ( 0.000000000000000000, 1.000000000000000000, 0.000000000000000000 ) ) ;
#318 = DIRECTION ( 'NONE',  ( -0.000000000000000000, -1.000000000000000000, -0.000000000000000000 ) ) ;
#319 = CARTESIAN_POINT ( 'NONE',  ( 1.613287804444627715, 0.05773177243535584924, 0.4772134490897159131 ) ) ;
#320 = AXIS2_PLACEMENT_3D ( 'NONE', #8571, #13282, #12223 ) ;
#321 =( CONVERSION_BASED_UNIT ( 'INCH', #9691 ) LENGTH_UNIT ( ) NAMED_UNIT ( #8723 ) );
#322 = DIRECTION ( 'NONE',  ( -0.000000000000000000, -1.000000000000000000, -0.000000000000000000 ) ) ;
#323 = DIRECTION ( 'NONE',  ( 0.000000000000000000, 0.000000000000000000, 1.000000000000000000 ) ) ;
#324 = ADVANCED_FACE ( 'NONE', ( #14504 ), #6670, .F. ) ;
#325 = ADVANCED_FACE ( 'NONE', ( #5492 ), #796, .F. ) ;
#326 = CARTESIAN_POINT ( 'NONE',  ( 4.309703551682574130, 1.729087785011442335, -0.6133796147049294101 ) ) ;
#327 = VERTEX_POINT ( 'NONE', #12220 ) ;
#329 = ORIENTED_EDGE ( 'NONE', *, *, #1473, .T. ) ;
#328 = DIRECTION ( 'NONE',  ( 0.000000000000000000, 0.000000000000000000, 1.000000000000000000 ) ) ;
#330 = CIRCLE ( 'NONE', #3785, 2.500000000000000444 ) ;
#331 = VERTEX_POINT ( 'NONE', #646 ) ;
#332 = DIRECTION ( 'NONE',  ( 0.000000000000000000, 0.000000000000000000, 1.000000000000000000 ) ) ;
#333 = AXIS2_PLACEMENT_3D ( 'NONE', #4078, #9892, #14552 ) ;
#334 = CIRCLE ( 'NONE', #14035, 2.000179419058113695 ) ;
#335 = CARTESIAN_POINT ( 'NONE',  ( 3.426491571325181340, -2.360000000000016751, -0.9799999999999431388 ) ) ;
#336 = APPLICATION_PROTOCOL_DEFINITION ( 'draft international standard', 'automotive_design', 1998, #3426 ) ;
#337 = CARTESIAN_POINT ( 'NONE',  ( 3.426491571325181340, 0.000000000000000000, 0.000000000000000000 ) ) ;
#338 = ORIENTED_EDGE ( 'NONE', *, *, #2110, .F. ) ;
#339 = DIRECTION ( 'NONE',  ( 0.7071067811865551223, 0.000000000000000000, -0.7071067811865400232 ) ) ;
#340 = DIRECTION ( 'NONE',  ( -1.000000000000000000, 0.000000000000000000, 0.000000000000000000 ) ) ;
#341 = ADVANCED_FACE ( 'NONE', ( #14586 ), #4119, .F. ) ;
#342 = DIRECTION ( 'NONE',  ( -0.7071067811865406894, 0.000000000000000000, 0.7071067811865542341 ) ) ;
#343 = EDGE_CURVE ( 'NONE', #4313, #8918, #8861, .T. ) ;
#344 = CIRCLE ( 'NONE', #11853, 2.500000000000000444 ) ;
#345 = DIRECTION ( 'NONE',  ( 0.000000000000000000, 0.000000000000000000, -1.000000000000000000 ) ) ;
#346 = VECTOR ( 'NONE', #13242, 39.37007874015748143 ) ;
#347 = AXIS2_PLACEMENT_3D ( 'NONE', #11254, #8885, #14698 ) ;
#348 = DIRECTION ( 'NONE',  ( 0.8660254037844387076, 0.000000000000000000, 0.4999999999999999445 ) ) ;
#349 = CARTESIAN_POINT ( 'NONE',  ( 3.707746441153773720, 1.919327537284637453, 0.7315114958933836009 ) ) ;
#350 = DIRECTION ( 'NONE',  ( 0.000000000000000000, 1.000000000000000000, 0.000000000000000000 ) ) ;
#351 = ORIENTED_EDGE ( 'NONE', *, *, #3241, .T. ) ;
#352 = DIRECTION ( 'NONE',  ( 1.000000000000000000, 0.000000000000000000, 0.000000000000000000 ) ) ;
#354 = ORIENTED_EDGE ( 'NONE', *, *, #6727, .F. ) ;
#353 = DIRECTION ( 'NONE',  ( 0.000000000000000000, 0.000000000000000000, 1.000000000000000000 ) ) ;
#355 = VERTEX_POINT ( 'NONE', #1882 ) ;
#356 = EDGE_CURVE ( 'NONE', #5312, #13169, #5450, .T. ) ;
#357 = CARTESIAN_POINT ( 'NONE',  ( 1.000000000000000222, -0.3829999999999998961, -0.4258697216429003785 ) ) ;
#358 = VECTOR ( 'NONE', #10511, 39.37007874015748143 ) ;
#359 = CARTESIAN_POINT ( 'NONE',  ( 3.601417382415921686, 0.9969999999999999973, 0.3891265382754439117 ) ) ;
#360 = EDGE_LOOP ( 'NONE', ( #2788, #10549, #4637, #1852 ) ) ;
#361 = FACE_OUTER_BOUND ( 'NONE', #10619, .T. ) ;
#362 = AXIS2_PLACEMENT_3D ( 'NONE', #8874, #4935, #7723 ) ;
#363 = AXIS2_PLACEMENT_3D ( 'NONE', #408, #6258, #3029 ) ;
#364 = EDGE_CURVE ( 'NONE', #2708, #7869, #8176, .T. ) ;
#365 = EDGE_CURVE ( 'NONE', #9131, #9822, #10086, .T. ) ;
#366 = CARTESIAN_POINT ( 'NONE',  ( 0.6844575745811053435, -0.004403083989539873129, 0.4560057122456970258 ) ) ;
#367 = DIRECTION ( 'NONE',  ( -0.000000000000000000, -1.000000000000000000, -0.000000000000000000 ) ) ;
#368 = ORIENTED_EDGE ( 'NONE', *, *, #14078, .F. ) ;
#369 = DIRECTION ( 'NONE',  ( 0.000000000000000000, 0.000000000000000000, -1.000000000000000000 ) ) ;
#370 = CARTESIAN_POINT ( 'NONE',  ( 0.000000000000000000, 0.000000000000000000, 1.000000000000000000 ) ) ;
#371 = AXIS2_PLACEMENT_3D ( 'NONE', #3600, #13748, #12921 ) ;
#372 = LINE ( 'NONE', #5149, #13869 ) ;
#373 = CIRCLE ( 'NONE', #2836, 0.05999999999999996309 ) ;
#374 = ORIENTED_EDGE ( 'NONE', *, *, #6094, .F. ) ;
#375 = DIRECTION ( 'NONE',  ( -1.000000000000000000, -0.000000000000000000, 0.000000000000000000 ) ) ;
#376 = CARTESIAN_POINT ( 'NONE',  ( 4.769268701363833074, 3.137999999999999901, -0.3249191361593797289 ) ) ;
#377 = EDGE_LOOP ( 'NONE', ( #1901, #13992, #9857, #660 ) ) ;
#378 = CARTESIAN_POINT ( 'NONE',  ( 1.552356239822776596, 2.176428591712472865E-16, 0.4178403161916762754 ) ) ;
#379 = ORIENTED_EDGE ( 'NONE', *, *, #8504, .T. ) ;
#380 = CARTESIAN_POINT ( 'NONE',  ( 2.124999999999999556, 0.000000000000000000, 0.000000000000000000 ) ) ;
#381 = AXIS2_PLACEMENT_3D ( 'NONE', #11771, #13044, #15132 ) ;
#382 = LINE ( 'NONE', #600, #11482 ) ;
#383 = EDGE_CURVE ( 'NONE', #2919, #710, #5448, .T. ) ;
#384 = DIRECTION ( 'NONE',  ( -1.000000000000000000, -0.000000000000000000, -0.000000000000000000 ) ) ;
#385 = CIRCLE ( 'NONE', #8720, 0.4349999999999999978 ) ;
#386 = FACE_OUTER_BOUND ( 'NONE', #3561, .T. ) ;
#387 = DIRECTION ( 'NONE',  ( 0.000000000000000000, 1.000000000000000000, 0.000000000000000000 ) ) ;
#388 = DIMENSIONAL_EXPONENTS ( 1.000000000000000000, 0.000000000000000000, 0.000000000000000000, 0.000000000000000000, 0.000000000000000000, 0.000000000000000000, 0.000000000000000000 ) ;
#389 = VECTOR ( 'NONE', #6867, 39.37007874015748854 ) ;
#390 = ORIENTED_EDGE ( 'NONE', *, *, #14172, .T. ) ;
#391 = VERTEX_POINT ( 'NONE', #5798 ) ;
#392 = VERTEX_POINT ( 'NONE', #12587 ) ;
#393 = CARTESIAN_POINT ( 'NONE',  ( 8.792093969802149189, 0.8799778768672790186, 6.829619984160658046E-17 ) ) ;
#394 = DIRECTION ( 'NONE',  ( 0.000000000000000000, 0.000000000000000000, -1.000000000000000000 ) ) ;
#395 = CARTESIAN_POINT ( 'NONE',  ( 0.000000000000000000, 1.000000000000000000, 0.000000000000000000 ) ) ;
#396 = DIRECTION ( 'NONE',  ( -1.365923996832131609E-16, 1.000000000000000000, -0.000000000000000000 ) ) ;
#397 = CARTESIAN_POINT ( 'NONE',  ( 8.849999999999999645, 0.9399413264884247665, 6.829619984160658046E-17 ) ) ;
#398 = VECTOR ( 'NONE', #13183, 39.37007874015748143 ) ;
#399 = CARTESIAN_POINT ( 'NONE',  ( 4.330797523564109852, 1.779041412359303020, -0.5988230613860490159 ) ) ;
#400 = DIRECTION ( 'NONE',  ( -0.000000000000000000, 1.000000000000000000, 1.224646799147353207E-16 ) ) ;
#401 = AXIS2_PLACEMENT_3D ( 'NONE', #14432, #9845, #14497 ) ;
#402 = CARTESIAN_POINT ( 'NONE',  ( 4.468111723579847983, 1.731463736471003267, -0.4625016237982221279 ) ) ;
#403 = ORIENTED_EDGE ( 'NONE', *, *, #4180, .F. ) ;
#404 = ORIENTED_EDGE ( 'NONE', *, *, #6402, .T. ) ;
#405 = ORIENTED_EDGE ( 'NONE', *, *, #14962, .F. ) ;
#406 = DIRECTION ( 'NONE',  ( -0.000000000000000000, 1.000000000000000000, 1.224646799147353207E-16 ) ) ;
#407 = DIRECTION ( 'NONE',  ( 0.000000000000000000, 0.000000000000000000, -1.000000000000000000 ) ) ;
#409 = AXIS2_PLACEMENT_3D ( 'NONE', #164, #4937, #14245 ) ;
#408 = CARTESIAN_POINT ( 'NONE',  ( 6.176491571325181340, 1.679378605318059492, 1.679378605318041506 ) ) ;
#410 = CARTESIAN_POINT ( 'NONE',  ( 2.156999999999999584, 1.679378605318042395, -1.941878605318058115 ) ) ;
#411 = EDGE_LOOP ( 'NONE', ( #4478, #9500, #8078, #9517 ) ) ;
#412 = CARTESIAN_POINT ( 'NONE',  ( 6.826491571325181695, -1.679378605318048390, 2.054378605318054607 ) ) ;
#413 = DIRECTION ( 'NONE',  ( 0.000000000000000000, 0.000000000000000000, 1.000000000000000000 ) ) ;
#414 = EDGE_CURVE ( 'NONE', #6236, #10807, #12035, .T. ) ;
#415 = AXIS2_PLACEMENT_3D ( 'NONE', #5979, #1448, #8366 ) ;
#416 = ADVANCED_FACE ( 'NONE', ( #11763 ), #6950, .T. ) ;
#417 = DIRECTION ( 'NONE',  ( -0.000000000000000000, -1.000000000000000000, -0.000000000000000000 ) ) ;
#418 = ADVANCED_FACE ( 'NONE', ( #3344 ), #2756, .F. ) ;
#419 = FACE_BOUND ( 'NONE', #11728, .T. ) ;
#420 = CIRCLE ( 'NONE', #5332, 0.4849999999999999312 ) ;
#421 = CARTESIAN_POINT ( 'NONE',  ( 0.8032009730227706035, -0.4429999999999999494, -0.4342979540647063930 ) ) ;
#422 = EDGE_CURVE ( 'NONE', #10962, #11613, #2463, .T. ) ;
#423 = DIRECTION ( 'NONE',  ( 0.000000000000000000, 0.000000000000000000, -1.000000000000000000 ) ) ;
#424 = CARTESIAN_POINT ( 'NONE',  ( 3.779260009907372098, 1.809000757605977894, 0.7955663742672792749 ) ) ;
#425 = CARTESIAN_POINT ( 'NONE',  ( 2.774999999999999911, -1.679378605318041950, 1.679378605318059048 ) ) ;
#426 = ORIENTED_EDGE ( 'NONE', *, *, #1651, .T. ) ;
#427 = CARTESIAN_POINT ( 'NONE',  ( 2.124999999999999556, 0.9800000000000039790, 3.360000000000000320 ) ) ;
#429 = ORIENTED_EDGE ( 'NONE', *, *, #6348, .F. ) ;
#428 = FACE_BOUND ( 'NONE', #2478, .T. ) ;
#430 = CIRCLE ( 'NONE', #4372, 1.999999999999999334 ) ;
#431 = ORIENTED_EDGE ( 'NONE', *, *, #11597, .T. ) ;
#432 = VECTOR ( 'NONE', #14989, 39.37007874015748143 ) ;
#433 = CIRCLE ( 'NONE', #15106, 0.5000000000000001110 ) ;
#434 = DIRECTION ( 'NONE',  ( 0.000000000000000000, 0.000000000000000000, 1.000000000000000000 ) ) ;
#435 = CARTESIAN_POINT ( 'NONE',  ( 3.426491571325181340, 2.360000000000015863, 1.574999999999999956 ) ) ;
#436 = VERTEX_POINT ( 'NONE', #1191 ) ;
#437 = CIRCLE ( 'NONE', #2657, 0.1000000000000000194 ) ;
#438 = CARTESIAN_POINT ( 'NONE',  ( 0.000000000000000000, 1.249999999999999778, 0.000000000000000000 ) ) ;
#439 = AXIS2_PLACEMENT_3D ( 'NONE', #4419, #13876, #8096 ) ;
#440 = CIRCLE ( 'NONE', #11957, 0.7849999999999996980 ) ;
#441 = CARTESIAN_POINT ( 'NONE',  ( 0.6766938413713005085, 0.03160638642086351091, 0.4478646436804253339 ) ) ;
#442 = VECTOR ( 'NONE', #5367, 39.37007874015748143 ) ;
#443 = LINE ( 'NONE', #1679, #13645 ) ;
#444 = ORIENTED_EDGE ( 'NONE', *, *, #8806, .T. ) ;
#445 = AXIS2_PLACEMENT_3D ( 'NONE', #7590, #1692, #9968 ) ;
#446 = LINE ( 'NONE', #2921, #8765 ) ;
#447 = FACE_OUTER_BOUND ( 'NONE', #360, .T. ) ;
#448 = FACE_OUTER_BOUND ( 'NONE', #12958, .T. ) ;
#449 = ADVANCED_FACE ( 'NONE', ( #9398 ), #8141, .F. ) ;
#450 = ORIENTED_EDGE ( 'NONE', *, *, #13190, .T. ) ;
#451 = VECTOR ( 'NONE', #6623, 39.37007874015748143 ) ;
#452 = CARTESIAN_POINT ( 'NONE',  ( 3.426491571325181340, 3.137999999999999901, -0.2209981660730358233 ) ) ;
#453 = ORIENTED_EDGE ( 'NONE', *, *, #4195, .F. ) ;
#454 = ADVANCED_FACE ( 'NONE', ( #14039 ), #12817, .T. ) ;
#455 = DIRECTION ( 'NONE',  ( 1.000000000000000000, 0.000000000000000000, 0.000000000000000000 ) ) ;
#456 = ORIENTED_EDGE ( 'NONE', *, *, #5293, .T. ) ;
#457 = ADVANCED_FACE ( 'NONE', ( #2193 ), #10309, .T. ) ;
#458 = DIRECTION ( 'NONE',  ( -0.000000000000000000, 1.000000000000000000, -0.000000000000000000 ) ) ;
#459 = CIRCLE ( 'NONE', #8798, 0.4070000000000022489 ) ;
#460 = DIRECTION ( 'NONE',  ( 0.000000000000000000, 0.000000000000000000, -1.000000000000000000 ) ) ;
#461 = CARTESIAN_POINT ( 'NONE',  ( 2.156999999999999140, -1.679378605318041950, 1.941878605318059003 ) ) ;
#462 = DIRECTION ( 'NONE',  ( 0.000000000000000000, 0.000000000000000000, -1.000000000000000000 ) ) ;
#463 = CARTESIAN_POINT ( 'NONE',  ( 1.936801488370565982, 0.2309360081137091791, -0.4726440467746176877 ) ) ;
#464 = ORIENTED_EDGE ( 'NONE', *, *, #6124, .F. ) ;
#465 = ORIENTED_EDGE ( 'NONE', *, *, #5796, .T. ) ;
#466 = ORIENTED_EDGE ( 'NONE', *, *, #11100, .T. ) ;
#467 = AXIS2_PLACEMENT_3D ( 'NONE', #10705, #1433, #10781 ) ;
#468 = EDGE_CURVE ( 'NONE', #14590, #193, #2006, .T. ) ;
#469 = FACE_OUTER_BOUND ( 'NONE', #14095, .T. ) ;
#470 = CARTESIAN_POINT ( 'NONE',  ( 3.426491571325181340, 0.000000000000000000, 2.500000000000000444 ) ) ;
#471 = CARTESIAN_POINT ( 'NONE',  ( 3.394491571325183088, -1.679378605318041950, 1.941878605318059003 ) ) ;
#472 = FACE_OUTER_BOUND ( 'NONE', #6050, .T. ) ;
#473 = CARTESIAN_POINT ( 'NONE',  ( 2.650000000000001688, 1.224646799147353207E-16, 1.000000000000000000 ) ) ;
#474 = CARTESIAN_POINT ( 'NONE',  ( 4.041559342806273492, 1.811112142523843005, 0.7320156718295878218 ) ) ;
#475 = CARTESIAN_POINT ( 'NONE',  ( 4.249538226556600407, 1.782304664937925498, -0.6509308308851882163 ) ) ;
#476 = ORIENTED_EDGE ( 'NONE', *, *, #8664, .T. ) ;
#477 = EDGE_LOOP ( 'NONE', ( #13690, #3186, #11488, #1344 ) ) ;
#478 = ORIENTED_EDGE ( 'NONE', *, *, #3162, .F. ) ;
#479 = TOROIDAL_SURFACE ( 'NONE', #243, 0.7057575716915831521, 0.04000000000000000083 ) ;
#480 = CARTESIAN_POINT ( 'NONE',  ( 0.01817859877509219249, 1.603284996591855194, 0.3809527529760087239 ) ) ;
#481 = ADVANCED_FACE ( 'NONE', ( #9320 ), #2760, .F. ) ;
#482 = DIMENSIONAL_EXPONENTS ( 1.000000000000000000, 0.000000000000000000, 0.000000000000000000, 0.000000000000000000, 0.000000000000000000, 0.000000000000000000, 0.000000000000000000 ) ;
#483 = CARTESIAN_POINT ( 'NONE',  ( 1.863568193433660758, 0.06187774891384346942, -0.4736784153469822400 ) ) ;
#484 = CARTESIAN_POINT ( 'NONE',  ( 6.208491571325183145, 1.679378605318059492, 1.304378605318041062 ) ) ;
#485 = CARTESIAN_POINT ( 'NONE',  ( 3.470516203623992713, 1.056999999999999718, 0.3909199583802897005 ) ) ;
#486 = ORIENTED_EDGE ( 'NONE', *, *, #13237, .F. ) ;
#487 =( BOUNDED_CURVE ( )  B_SPLINE_CURVE ( 3, ( #249, #9614, #6464, #3179 ),
 .UNSPECIFIED., .F., .T. ) 
 B_SPLINE_CURVE_WITH_KNOTS ( ( 4, 4 ),
 ( 1.570796326794896558, 2.356194490192347057 ),
 .UNSPECIFIED. ) 
 CURVE ( )  GEOMETRIC_REPRESENTATION_ITEM ( )  RATIONAL_B_SPLINE_CURVE ( ( 1.000000000000000000, 0.9492530216741907889, 0.9492530216741907889, 1.000000000000000000 ) ) 
 REPRESENTATION_ITEM ( '' )  );
#488 = CYLINDRICAL_SURFACE ( 'NONE', #3122, 1.350000000000000089 ) ;
#489 = CARTESIAN_POINT ( 'NONE',  ( 2.774999999999999911, -1.679378605318041950, 1.941878605318059003 ) ) ;
#490 = DIRECTION ( 'NONE',  ( -1.000000000000000000, -1.578435611247398256E-16, 0.000000000000000000 ) ) ;
#491 = MANIFOLD_SOLID_BREP ( 'Chamfer5', #14246 ) ;
#492 = AXIS2_PLACEMENT_3D ( 'NONE', #3318, #11420, #3396 ) ;
#493 = PLANE ( 'NONE',  #11640 ) ;
#494 = CARTESIAN_POINT ( 'NONE',  ( 0.09035531712817643224, 1.379999999999999671, 0.1564999999999999447 ) ) ;
#495 = CARTESIAN_POINT ( 'NONE',  ( 3.370072511834198981, 1.982174769829836869, 0.6499189952005048898 ) ) ;
#496 = ADVANCED_FACE ( 'NONE', ( #104 ), #9163, .F. ) ;
#498 = VERTEX_POINT ( 'NONE', #4806 ) ;
#497 = DIRECTION ( 'NONE',  ( -1.000000000000000000, -0.000000000000000000, -0.000000000000000000 ) ) ;
#499 = EDGE_CURVE ( 'NONE', #1229, #14925, #2522, .T. ) ;
#500 = ORIENTED_EDGE ( 'NONE', *, *, #14271, .T. ) ;
#501 = EDGE_CURVE ( 'NONE', #1342, #114, #5947, .T. ) ;
#502 = DIRECTION ( 'NONE',  ( 1.000000000000000000, 0.000000000000000000, 0.000000000000000000 ) ) ;
#504 = VERTEX_POINT ( 'NONE', #9475 ) ;
#503 = PLANE ( 'NONE',  #14800 ) ;
#505 = EDGE_LOOP ( 'NONE', ( #7717, #2716, #8517, #10389 ) ) ;
#506 = CARTESIAN_POINT ( 'NONE',  ( 0.06299999999999998657, 0.000000000000000000, -1.875500000000000167 ) ) ;
#507 = LENGTH_MEASURE_WITH_UNIT ( LENGTH_MEASURE( 0.02539999999999999897 ), #1669 );
#508 = DIRECTION ( 'NONE',  ( -1.000000000000000000, -0.000000000000000000, -0.000000000000000000 ) ) ;
#509 = EDGE_LOOP ( 'NONE', ( #10431, #1646, #3690, #10294 ) ) ;
#510 = CIRCLE ( 'NONE', #6642, 1.000000000000000000 ) ;
#511 = CARTESIAN_POINT ( 'NONE',  ( 2.124999999999999556, -1.679378605318059048, -1.384878605318057510 ) ) ;
#512 = DIRECTION ( 'NONE',  ( 0.000000000000000000, 0.000000000000000000, 1.000000000000000000 ) ) ;
#513 = ADVANCED_FACE ( 'NONE', ( #3662 ), #8439, .T. ) ;
#514 = CARTESIAN_POINT ( 'NONE',  ( 0.5400755080658357077, 0.1749999999999999889, -1.657626322880899616 ) ) ;
#515 = DIRECTION ( 'NONE',  ( 1.000000000000000000, 0.000000000000000000, 0.000000000000000000 ) ) ;
#516 = ORIENTED_EDGE ( 'NONE', *, *, #4824, .F. ) ;
#517 = CARTESIAN_POINT ( 'NONE',  ( -0.4124999999999999223, 0.1749999999999999889, 0.3724999999999999978 ) ) ;
#518 = CARTESIAN_POINT ( 'NONE',  ( 2.774999999999999911, 2.360000000000016307, 0.9799999999999454703 ) ) ;
#519 = EDGE_CURVE ( 'NONE', #6687, #3130, #2785, .T. ) ;
#520 = SURFACE_SIDE_STYLE ('',( #1685 ) ) ;
#521 = EDGE_LOOP ( 'NONE', ( #12899, #4880, #11029, #14009, #13965, #2995, #9899, #2358 ) ) ;
#522 = PRODUCT_DEFINITION_SHAPE ( 'NONE', 'NONE',  #15160 ) ;
#523 = DIRECTION ( 'NONE',  ( 0.000000000000000000, 0.000000000000000000, -1.000000000000000000 ) ) ;
#524 = VERTEX_POINT ( 'NONE', #1618 ) ;
#525 = CARTESIAN_POINT ( 'NONE',  ( -0.2324505233676816274, 1.569549437900772393, 0.3592893892332145733 ) ) ;
#526 = ORIENTED_EDGE ( 'NONE', *, *, #5349, .F. ) ;
#527 = AXIS2_PLACEMENT_3D ( 'NONE', #12711, #14236, #2546 ) ;
#528 = CARTESIAN_POINT ( 'NONE',  ( 1.831696981322115780, 0.1157067236523833115, -0.4136843993219123106 ) ) ;
#529 = EDGE_CURVE ( 'NONE', #6474, #14724, #5304, .T. ) ;
#530 = CARTESIAN_POINT ( 'NONE',  ( 3.426491571325181340, -1.679378605318041950, 1.679378605318059048 ) ) ;
#531 = DIRECTION ( 'NONE',  ( 1.000000000000000000, 0.000000000000000000, 0.000000000000000000 ) ) ;
#532 = EDGE_CURVE ( 'NONE', #2140, #9681, #11301, .T. ) ;
#533 = LINE ( 'NONE', #9820, #5247 ) ;
#534 = DIRECTION ( 'NONE',  ( 0.000000000000000000, 1.000000000000000000, 0.000000000000000000 ) ) ;
#535 = ORIENTED_EDGE ( 'NONE', *, *, #1965, .T. ) ;
#536 = ORIENTED_EDGE ( 'NONE', *, *, #13800, .F. ) ;
#537 = ORIENTED_EDGE ( 'NONE', *, *, #1029, .F. ) ;
#538 = CARTESIAN_POINT ( 'NONE',  ( 8.849999999999999645, 0.9399413264884969310, -0.04934655444149117082 ) ) ;
#539 = VERTEX_POINT ( 'NONE', #3171 ) ;
#540 = CIRCLE ( 'NONE', #13989, 1.000000000000000000 ) ;
#541 = CARTESIAN_POINT ( 'NONE',  ( 3.426491571325181340, 0.000000000000000000, 0.000000000000000000 ) ) ;
#542 = DIRECTION ( 'NONE',  ( 1.000000000000000000, 0.000000000000000000, 0.000000000000000000 ) ) ;
#543 = CARTESIAN_POINT ( 'NONE',  ( 8.849999999999999645, 0.9399413264884247665, -0.2203075555454639678 ) ) ;
#544 = CARTESIAN_POINT ( 'NONE',  ( 4.329246711911844514, 1.779530689460202320, 0.5984961127851674556 ) ) ;
#545 = EDGE_CURVE ( 'NONE', #3991, #4965, #11057, .T. ) ;
#546 = EDGE_CURVE ( 'NONE', #1773, #10754, #10215, .T. ) ;
#547 = DIRECTION ( 'NONE',  ( -1.000000000000000000, 0.000000000000000000, 1.655665450705613915E-16 ) ) ;
#548 = CIRCLE ( 'NONE', #11077, 1.000000000000000222 ) ;
#549 = CLOSED_SHELL ( 'NONE', ( #5488, #481, #7292, #11440, #11908, #9531, #3714, #2619, #5887, #8436, #6105, #1471, #8156, #11332, #12780, #2405, #7263, #14183, #6009, #11214, #11092, #1051, #416, #12347, #10729, #6027, #11234, #7644, #7915, #5914, #9798, #14421, #14956, #1945, #6230, #12029, #9162, #10430, #15014, #657, #3349, #12038, #13659, #9739, #6270, #8151, #13249, #11391, #1877, #5212, #513, #12775, #1170, #13088, #4368, #635, #8400, #12740, #13598, #8336, #7884, #9967, #8541, #15045, #9982, #13065, #14395, #8709, #14079, #13106, #14372, #2783, #2220, #12247, #8585, #5823, #14354, #7669, #4557, #4229, #14131, #8678, #8076, #2011, #13221, #15022, #8482, #2314, #278, #1941, #10668 ) ) ;
#550 = EDGE_LOOP ( 'NONE', ( #3522, #12359, #5503, #368 ) ) ;
#551 = EDGE_LOOP ( 'NONE', ( #6863, #3717, #2455, #3329 ) ) ;
#552 = ORIENTED_EDGE ( 'NONE', *, *, #11125, .T. ) ;
#553 = DIRECTION ( 'NONE',  ( -1.000000000000000000, -1.365923996832131609E-16, 0.000000000000000000 ) ) ;
#554 = DIRECTION ( 'NONE',  ( 0.000000000000000000, 0.000000000000000000, 1.000000000000000000 ) ) ;
#555 = CARTESIAN_POINT ( 'NONE',  ( 3.426491571325181340, 1.679378605318059048, 1.679378605318041506 ) ) ;
#556 = CARTESIAN_POINT ( 'NONE',  ( 2.956986065683078202, 0.9548522091760921482, 0.3979556114002301137 ) ) ;
#557 = VERTEX_POINT ( 'NONE', #11417 ) ;
#558 = AXIS2_PLACEMENT_3D ( 'NONE', #7883, #12612, #2053 ) ;
#559 = CARTESIAN_POINT ( 'NONE',  ( 3.875000000000000000, 3.137999999999999901, -0.5174999999999995159 ) ) ;
#560 = DIRECTION ( 'NONE',  ( 0.000000000000000000, -1.000000000000000000, 0.000000000000000000 ) ) ;
#561 = AXIS2_PLACEMENT_3D ( 'NONE', #967, #4507, #4584 ) ;
#562 = LINE ( 'NONE', #7784, #9750 ) ;
#563 = ADVANCED_FACE ( 'NONE', ( #6763 ), #8985, .F. ) ;
#564 = DIRECTION ( 'NONE',  ( -0.000000000000000000, -0.000000000000000000, 1.000000000000000000 ) ) ;
#565 = CARTESIAN_POINT ( 'NONE',  ( 0.9125303617078899254, -0.4616528667627542992, -0.4492488068439366988 ) ) ;
#566 = CIRCLE ( 'NONE', #9416, 2.500000000000000444 ) ;
#567 = CARTESIAN_POINT ( 'NONE',  ( 4.418784802593074268, 1.729109169374164923, 0.5194219853913167873 ) ) ;
#569 = EDGE_LOOP ( 'NONE', ( #13025, #1220 ) ) ;
#568 = CARTESIAN_POINT ( 'NONE',  ( 0.7067472695984848841, -0.3830000000000000071, 0.5500236785040136800 ) ) ;
#570 = ORIENTED_EDGE ( 'NONE', *, *, #28, .T. ) ;
#571 = CARTESIAN_POINT ( 'NONE',  ( -0.3930894239865136974, 1.593697031032158318, -0.08105465168939116061 ) ) ;
#573 = ORIENTED_EDGE ( 'NONE', *, *, #1982, .T. ) ;
#572 = DIRECTION ( 'NONE',  ( 1.000000000000000000, 0.000000000000000000, 0.000000000000000000 ) ) ;
#574 =( BOUNDED_CURVE ( )  B_SPLINE_CURVE ( 3, ( #13959, #7028, #11687, #3578 ),
 .UNSPECIFIED., .F., .F. ) 
 B_SPLINE_CURVE_WITH_KNOTS ( ( 4, 4 ),
 ( 3.926990816987246724, 4.712388980384689674 ),
 .UNSPECIFIED. ) 
 CURVE ( )  GEOMETRIC_REPRESENTATION_ITEM ( )  RATIONAL_B_SPLINE_CURVE ( ( 1.000000000000000000, 0.9492530216741918991, 0.9492530216741918991, 1.000000000000000000 ) ) 
 REPRESENTATION_ITEM ( '' )  );
#575 = ORIENTED_EDGE ( 'NONE', *, *, #5776, .F. ) ;
#576 = CARTESIAN_POINT ( 'NONE',  ( 0.6766651500320096657, 0.03157991788063375938, 0.4479228816209581687 ) ) ;
#577 = CARTESIAN_POINT ( 'NONE',  ( 2.742999999999999883, -1.679378605318041950, 1.941878605318059003 ) ) ;
#578 = ORIENTED_EDGE ( 'NONE', *, *, #9901, .F. ) ;
#579 = CYLINDRICAL_SURFACE ( 'NONE', #362, 0.06000000000000021982 ) ;
#580 = CARTESIAN_POINT ( 'NONE',  ( 2.743000000000000771, 1.679378605318059048, 1.416878605318041773 ) ) ;
#581 = VECTOR ( 'NONE', #5660, 39.37007874015748143 ) ;
#582 = EDGE_CURVE ( 'NONE', #6020, #5479, #13980, .T. ) ;
#583 = AXIS2_PLACEMENT_3D ( 'NONE', #12548, #3233, #6611 ) ;
#584 = AXIS2_PLACEMENT_3D ( 'NONE', #12545, #6758, #756 ) ;
#585 = LINE ( 'NONE', #514, #7696 ) ;
#586 = DIRECTION ( 'NONE',  ( 1.000000000000000000, 0.000000000000000000, 0.000000000000000000 ) ) ;
#587 = VERTEX_POINT ( 'NONE', #15009 ) ;
#588 = CARTESIAN_POINT ( 'NONE',  ( 2.980731298636167370, 3.137999999999999901, 0.3249191361593796734 ) ) ;
#589 = LINE ( 'NONE', #1684, #13235 ) ;
#590 = PRESENTATION_STYLE_ASSIGNMENT (( #6371 ) ) ;
#591 = ORIENTED_EDGE ( 'NONE', *, *, #11529, .T. ) ;
#592 = CIRCLE ( 'NONE', #14054, 0.1000000000000000194 ) ;
#593 = DIRECTION ( 'NONE',  ( 0.000000000000000000, 0.000000000000000000, 1.000000000000000000 ) ) ;
#594 = DIRECTION ( 'NONE',  ( -0.000000000000000000, -1.000000000000000000, -0.000000000000000000 ) ) ;
#595 = EDGE_LOOP ( 'NONE', ( #450, #9611, #14713, #14999 ) ) ;
#596 = VECTOR ( 'NONE', #1390, 39.37007874015748143 ) ;
#597 = AXIS2_PLACEMENT_3D ( 'NONE', #8204, #9276, #13832 ) ;
#598 = DIRECTION ( 'NONE',  ( 0.000000000000000000, 0.000000000000000000, -1.000000000000000000 ) ) ;
#599 = ORIENTED_EDGE ( 'NONE', *, *, #9243, .T. ) ;
#600 = CARTESIAN_POINT ( 'NONE',  ( 2.775039370078740131, 1.679378605318035733, -1.304378605318064821 ) ) ;
#601 = EDGE_CURVE ( 'NONE', #8372, #9653, #8938, .T. ) ;
#602 = EDGE_CURVE ( 'NONE', #10522, #4605, #13769, .T. ) ;
#603 = VECTOR ( 'NONE', #10639, 39.37007874015748143 ) ;
#604 = CARTESIAN_POINT ( 'NONE',  ( 1.261796151055322168, -0.4301078242393397977, 0.4222829664659954463 ) ) ;
#605 = CARTESIAN_POINT ( 'NONE',  ( 2.124999999999999556, 0.000000000000000000, -1.875000000000000000 ) ) ;
#606 = ADVANCED_FACE ( 'NONE', ( #1000 ), #6674, .F. ) ;
#607 = CARTESIAN_POINT ( 'NONE',  ( 1.003096136995460075, -0.4429976034824905651, -0.4258273028168328977 ) ) ;
#608 = AXIS2_PLACEMENT_3D ( 'NONE', #2450, #9183, #10407 ) ;
#609 = AXIS2_PLACEMENT_3D ( 'NONE', #12044, #1552, #6237 ) ;
#610 = DIRECTION ( 'NONE',  ( -0.000000000000000000, -1.000000000000000000, -0.000000000000000000 ) ) ;
#611 = CARTESIAN_POINT ( 'NONE',  ( 1.250847373107696114, 9.390727478220904197E-17, -0.4823326642216427818 ) ) ;
#612 = ADVANCED_FACE ( 'NONE', ( #3391 ), #6846, .F. ) ;
#613 = DIRECTION ( 'NONE',  ( 0.000000000000000000, 0.000000000000000000, -1.000000000000000000 ) ) ;
#614 = ORIENTED_EDGE ( 'NONE', *, *, #2822, .T. ) ;
#615 = ORIENTED_EDGE ( 'NONE', *, *, #5487, .T. ) ;
#616 = VERTEX_POINT ( 'NONE', #7829 ) ;
#617 = EDGE_CURVE ( 'NONE', #3063, #2897, #6417, .T. ) ;
#618 = VECTOR ( 'NONE', #11913, 39.37007874015748854 ) ;
#619 = CARTESIAN_POINT ( 'NONE',  ( 8.775135155112147700, 0.9377394161891228208, -0.2318982201004599064 ) ) ;
#620 = ORIENTED_EDGE ( 'NONE', *, *, #7740, .F. ) ;
#621 = LINE ( 'NONE', #5395, #4023 ) ;
#622 = CARTESIAN_POINT ( 'NONE',  ( 0.6757896753473673357, -0.3817456040190621014, -0.4909021876970636744 ) ) ;
#623 = CARTESIAN_POINT ( 'NONE',  ( 2.774999999999999911, 1.575000000000000178, -2.360000000000016751 ) ) ;
#624 = CARTESIAN_POINT ( 'NONE',  ( 4.438984740194723777, 1.783484299094709291, -0.4967767970635435515 ) ) ;
#625 = AXIS2_PLACEMENT_3D ( 'NONE', #5408, #7774, #1867 ) ;
#626 = VERTEX_POINT ( 'NONE', #9128 ) ;
#627 = EDGE_CURVE ( 'NONE', #5452, #9898, #761, .T. ) ;
#628 = VERTEX_POINT ( 'NONE', #13626 ) ;
#629 = ORIENTED_EDGE ( 'NONE', *, *, #13918, .F. ) ;
#630 = ADVANCED_FACE ( 'NONE', ( #11500 ), #13727, .F. ) ;
#631 = ORIENTED_EDGE ( 'NONE', *, *, #11576, .F. ) ;
#632 = CARTESIAN_POINT ( 'NONE',  ( 0.2285544654201319137, 1.564824237736521129, -0.3660375595476001442 ) ) ;
#633 = FACE_OUTER_BOUND ( 'NONE', #11405, .T. ) ;
#634 = CARTESIAN_POINT ( 'NONE',  ( 4.098661581315266922, 0.8939497136434934044, 0.4483968163765176818 ) ) ;
#635 = ADVANCED_FACE ( 'NONE', ( #4537 ), #692, .T. ) ;
#636 = VECTOR ( 'NONE', #2663, 39.37007874015748143 ) ;
#637 = CARTESIAN_POINT ( 'NONE',  ( 2.742551415177972185, 0.8007359432430831703, 0.4612633980907066000 ) ) ;
#638 = VERTEX_POINT ( 'NONE', #10737 ) ;
#639 = CARTESIAN_POINT ( 'NONE',  ( 0.2849999999999999201, 0.000000000000000000, -0.4108223460329290533 ) ) ;
#640 = LINE ( 'NONE', #3962, #6834 ) ;
#641 = CARTESIAN_POINT ( 'NONE',  ( 6.176491571325181340, 3.649833176986403141E-16, 2.960629921259842146 ) ) ;
#642 = AXIS2_PLACEMENT_3D ( 'NONE', #1430, #11848, #4665 ) ;
#643 = PRODUCT_DEFINITION_SHAPE ( 'NONE', 'NONE',  #869 ) ;
#644 = CARTESIAN_POINT ( 'NONE',  ( 0.000000000000000000, 1.000000000000000000, -1.000000000000000000 ) ) ;
#645 = B_SPLINE_CURVE_WITH_KNOTS ( 'NONE', 3,
 ( #5114, #3957, #11218, #6479, #7618, #8623, #9772, #634, #9841, #5040, #5331, #10007, #13340, #2878, #7549, #14493, #3889, #13422, #2956, #9922, #9699, #4029, #8696, #12208, #8561, #7698, #6404, #12357, #11059, #13199, #14576, #2736, #7406, #4105, #9880, #13609, #674, #12244, #14844, #7658, #6597, #4066, #5288, #11097, #7885, #8734, #7585, #9962, #4298, #8966, #13528, #5376 ),
 .UNSPECIFIED., .F., .F.,
 ( 4, 2, 2, 2, 2, 2, 2, 2, 2, 2, 2, 2, 2, 2, 2, 2, 2, 2, 2, 2, 2, 2, 2, 2, 2, 4 ),
 ( 0.04039358074926006209, 0.04165364880998905645, 0.04291371687071805774, 0.04543385299217604645, 0.04795398911363403516, 0.04921405717436303645, 0.05047412523509203081, 0.05299426135654999870, 0.05425432941727896530, 0.05551439747800793884, 0.05803453359946587897, 0.05929460166019485945, 0.06055466972092382605, 0.06181473778165279959, 0.06307480584238177312, 0.06559494196383972020, 0.06685501002456870068, 0.06811507808529766728, 0.06937514614602664775, 0.07063521420675561435, 0.07315535032821354755, 0.07441541838894250027, 0.07567548644967146687, 0.07819562257112942782, 0.07945569063185840830, 0.08071575869258738878 ),
 .UNSPECIFIED. ) ;
#646 = CARTESIAN_POINT ( 'NONE',  ( 3.426491571325181340, -2.360000000000000320, 0.9799999999999999822 ) ) ;
#647 = CARTESIAN_POINT ( 'NONE',  ( 4.110025962911500130, 1.748120791446346800, 0.7137006213478416239 ) ) ;
#649 = ORIENTED_EDGE ( 'NONE', *, *, #7956, .F. ) ;
#648 = CARTESIAN_POINT ( 'NONE',  ( 3.573617713061139067, 1.991675394285061129, -0.3996246112651613003 ) ) ;
#650 = AXIS2_PLACEMENT_3D ( 'NONE', #530, #384, #3003 ) ;
#651 = VERTEX_POINT ( 'NONE', #8070 ) ;
#653 = EDGE_LOOP ( 'NONE', ( #4006, #1589, #12203, #1711 ) ) ;
#652 = DIRECTION ( 'NONE',  ( 0.000000000000000000, 1.000000000000000000, 0.000000000000000000 ) ) ;
#654 = ORIENTED_EDGE ( 'NONE', *, *, #7639, .T. ) ;
#655 = VECTOR ( 'NONE', #7061, 39.37007874015748143 ) ;
#656 = DIRECTION ( 'NONE',  ( -0.9999002670844991947, -0.000000000000000000, -0.01412288512831128343 ) ) ;
#657 = ADVANCED_FACE ( 'NONE', ( #1153 ), #3465, .T. ) ;
#658 = LENGTH_MEASURE_WITH_UNIT ( LENGTH_MEASURE( 0.02539999999999999897 ), #4132 );
#659 = CARTESIAN_POINT ( 'NONE',  ( 4.769268701363833074, 3.137999999999999901, -0.3249191361593797289 ) ) ;
#660 = ORIENTED_EDGE ( 'NONE', *, *, #12679, .F. ) ;
#661 = LINE ( 'NONE', #6081, #596 ) ;
#662 = CARTESIAN_POINT ( 'NONE',  ( 0.000000000000000000, 1.591999999999999638, -0.2812500000000000555 ) ) ;
#663 = AXIS2_PLACEMENT_3D ( 'NONE', #3116, #8851, #13492 ) ;
#664 = VECTOR ( 'NONE', #2691, 39.37007874015748854 ) ;
#665 = CARTESIAN_POINT ( 'NONE',  ( 3.426491571325181340, -2.360000000000016751, -0.9799999999999431388 ) ) ;
#666 = FACE_OUTER_BOUND ( 'NONE', #1064, .T. ) ;
#667 = ORIENTED_EDGE ( 'NONE', *, *, #11769, .T. ) ;
#668 = DIRECTION ( 'NONE',  ( 0.000000000000000000, 0.000000000000000000, -1.000000000000000000 ) ) ;
#669 = AXIS2_PLACEMENT_3D ( 'NONE', #11948, #9659, #8440 ) ;
#670 = CARTESIAN_POINT ( 'NONE',  ( 3.651563249442855597, 0.8939021589031062032, -0.4484876836904110875 ) ) ;
#671 = VECTOR ( 'NONE', #5225, 39.37007874015748143 ) ;
#672 = DIRECTION ( 'NONE',  ( -1.000000000000000000, -0.000000000000000000, -0.000000000000000000 ) ) ;
#673 = ORIENTED_EDGE ( 'NONE', *, *, #277, .F. ) ;
#674 = CARTESIAN_POINT ( 'NONE',  ( 4.271191871305239474, 0.9523025322212360644, -0.3054383546384628056 ) ) ;
#675 = CYLINDRICAL_SURFACE ( 'NONE', #1096, 0.5000000000000001110 ) ;
#676 = EDGE_LOOP ( 'NONE', ( #8791, #5902, #11091, #7043 ) ) ;
#677 = CIRCLE ( 'NONE', #9267, 0.1899999999999996136 ) ;
#678 = DIRECTION ( 'NONE',  ( -0.000000000000000000, -1.000000000000000000, -0.000000000000000000 ) ) ;
#679 = EDGE_LOOP ( 'NONE', ( #6399, #14772, #12515, #13247 ) ) ;
#680 = EDGE_CURVE ( 'NONE', #14399, #13316, #9442, .T. ) ;
#681 = FILL_AREA_STYLE ('',( #13534 ) ) ;
#682 = AXIS2_PLACEMENT_3D ( 'NONE', #12165, #221, #7367 ) ;
#683 = DIRECTION ( 'NONE',  ( 0.000000000000000000, -0.7071067811865500152, -0.7071067811865449082 ) ) ;
#684 = VECTOR ( 'NONE', #3368, 39.37007874015748143 ) ;
#685 = DIRECTION ( 'NONE',  ( 8.659560562354984627E-17, 0.7071067811865432429, -0.7071067811865516806 ) ) ;
#686 = AXIS2_PLACEMENT_3D ( 'NONE', #12659, #6869, #8926 ) ;
#687 = CARTESIAN_POINT ( 'NONE',  ( 0.9666012435391547752, -0.4437180647443542680, -0.4095160967654646877 ) ) ;
#688 = AXIS2_PLACEMENT_3D ( 'NONE', #8760, #9762, #10906 ) ;
#689 = ORIENTED_EDGE ( 'NONE', *, *, #4932, .F. ) ;
#690 = CIRCLE ( 'NONE', #4881, 0.06000000000000001860 ) ;
#691 = CARTESIAN_POINT ( 'NONE',  ( 0.8249999999999999556, -0.6230000000000016636, -0.3750000000000000555 ) ) ;
#692 = CYLINDRICAL_SURFACE ( 'NONE', #7165, 0.06000000000000001860 ) ;
#693 = CARTESIAN_POINT ( 'NONE',  ( 0.7058998964907862161, -0.3830000000000000071, -0.4900296624789436950 ) ) ;
#694 = VERTEX_POINT ( 'NONE', #6070 ) ;
#695 = ORIENTED_EDGE ( 'NONE', *, *, #1081, .T. ) ;
#696 = EDGE_CURVE ( 'NONE', #13169, #12132, #10427, .T. ) ;
#697 = EDGE_CURVE ( 'NONE', #587, #10371, #13969, .T. ) ;
#698 = LINE ( 'NONE', #7680, #4065 ) ;
#699 = ORIENTED_EDGE ( 'NONE', *, *, #10847, .T. ) ;
#700 = EDGE_CURVE ( 'NONE', #4913, #6255, #9520, .T. ) ;
#701 = AXIS2_PLACEMENT_3D ( 'NONE', #10499, #14927, #12704 ) ;
#702 = CARTESIAN_POINT ( 'NONE',  ( 0.3725000000000000533, 0.000000000000000000, 0.4124999999999999778 ) ) ;
#703 = CARTESIAN_POINT ( 'NONE',  ( 2.774999999999999911, 1.679378605318059048, 1.416878605318041773 ) ) ;
#704 = AXIS2_PLACEMENT_3D ( 'NONE', #13464, #8666, #8821 ) ;
#705 = FACE_OUTER_BOUND ( 'NONE', #12936, .T. ) ;
#706 = EDGE_CURVE ( 'NONE', #9538, #13964, #2311, .T. ) ;
#707 = CARTESIAN_POINT ( 'NONE',  ( 4.470587351505396434, 1.786057884980379873, 0.4605560640960539853 ) ) ;
#708 = ORIENTED_EDGE ( 'NONE', *, *, #10830, .F. ) ;
#709 = CIRCLE ( 'NONE', #222, 0.3750000000000007772 ) ;
#710 = VERTEX_POINT ( 'NONE', #11650 ) ;
#711 = ORIENTED_EDGE ( 'NONE', *, *, #8011, .F. ) ;
#712 = ORIENTED_EDGE ( 'NONE', *, *, #4651, .T. ) ;
#713 = CARTESIAN_POINT ( 'NONE',  ( 0.2667400994511441303, 1.593697031032149880, -0.2998981012866574480 ) ) ;
#714 = CARTESIAN_POINT ( 'NONE',  ( 6.176491571325181340, 1.934941942652818220E-16, 1.580000000000000071 ) ) ;
#715 = FACE_OUTER_BOUND ( 'NONE', #10174, .T. ) ;
#716 = DIRECTION ( 'NONE',  ( 0.000000000000000000, 0.000000000000000000, 1.000000000000000000 ) ) ;
#717 = ORIENTED_EDGE ( 'NONE', *, *, #6431, .T. ) ;
#718 = DIRECTION ( 'NONE',  ( 0.9743309173630049225, 0.2251205531944282245, 0.000000000000000000 ) ) ;
#719 = CARTESIAN_POINT ( 'NONE',  ( 0.4108223460329280541, 0.000000000000000000, 0.2850000000000013078 ) ) ;
#720 = CARTESIAN_POINT ( 'NONE',  ( 0.8999999999999998002, 0.1549999999999996103, -0.2949999999999999289 ) ) ;
#721 = FILL_AREA_STYLE_COLOUR ( '', #1983 ) ;
#722 = EDGE_CURVE ( 'NONE', #5214, #9310, #5440, .T. ) ;
#723 = FACE_OUTER_BOUND ( 'NONE', #3702, .T. ) ;
#724 = CARTESIAN_POINT ( 'NONE',  ( 0.9662251482428008131, -0.4440312122665854289, -0.4102559963803746323 ) ) ;
#725 = EDGE_CURVE ( 'NONE', #10222, #4107, #6183, .T. ) ;
#726 = VECTOR ( 'NONE', #13880, 39.37007874015748143 ) ;
#727 = CARTESIAN_POINT ( 'NONE',  ( 4.291638032986768714, 1.730033725795280697, 0.6249393708399010317 ) ) ;
#729 = ORIENTED_EDGE ( 'NONE', *, *, #3796, .F. ) ;
#728 = CARTESIAN_POINT ( 'NONE',  ( 3.874999999999999556, 3.105999999999998984, -1.130000000000000560 ) ) ;
#730 = ORIENTED_EDGE ( 'NONE', *, *, #6624, .F. ) ;
#732 = ORIENTED_EDGE ( 'NONE', *, *, #9430, .T. ) ;
#731 = DIRECTION ( 'NONE',  ( -0.000000000000000000, -1.000000000000000000, -0.000000000000000000 ) ) ;
#733 = VERTEX_POINT ( 'NONE', #9363 ) ;
#734 = CARTESIAN_POINT ( 'NONE',  ( 0.000000000000000000, 1.629999999999999893, 0.000000000000000000 ) ) ;
#735 =( NAMED_UNIT ( * ) SI_UNIT ( $, .STERADIAN. ) SOLID_ANGLE_UNIT ( ) );
#736 = FACE_OUTER_BOUND ( 'NONE', #7085, .T. ) ;
#737 = ORIENTED_EDGE ( 'NONE', *, *, #13348, .T. ) ;
#738 = DIRECTION ( 'NONE',  ( -1.000000000000000000, -0.000000000000000000, -0.000000000000000000 ) ) ;
#739 = CARTESIAN_POINT ( 'NONE',  ( 3.874999999999999556, 3.170500000000000096, 1.320000000000000062 ) ) ;
#740 = AXIS2_PLACEMENT_3D ( 'NONE', #2703, #375, #9368 ) ;
#741 = CARTESIAN_POINT ( 'NONE',  ( 2.715751415184352702, 0.8549853309854710259, -0.4616419291638462208 ) ) ;
#742 = DIRECTION ( 'NONE',  ( 0.000000000000000000, 0.000000000000000000, -1.000000000000000000 ) ) ;
#743 = ADVANCED_FACE ( 'NONE', ( #14005 ), #12943, .T. ) ;
#744 = ORIENTED_EDGE ( 'NONE', *, *, #2333, .F. ) ;
#745 = ADVANCED_FACE ( 'NONE', ( #14087 ), #226, .F. ) ;
#746 = CARTESIAN_POINT ( 'NONE',  ( 6.787121492585022509, 0.000000000000000000, -1.000000000000000000 ) ) ;
#747 = CARTESIAN_POINT ( 'NONE',  ( 3.490100261840733520, 1.973532854457274333, 0.3199934443535443207 ) ) ;
#748 = DIRECTION ( 'NONE',  ( 0.7071067811865446862, -0.7071067811865503483, 0.000000000000000000 ) ) ;
#749 = ORIENTED_EDGE ( 'NONE', *, *, #5402, .T. ) ;
#750 = DIRECTION ( 'NONE',  ( 0.7071067811865467956, 8.659560562354941486E-17, 0.7071067811865482389 ) ) ;
#751 = CARTESIAN_POINT ( 'NONE',  ( 1.650520655410188775, 0.000000000000000000, -0.5816197779170857451 ) ) ;
#752 = ORIENTED_EDGE ( 'NONE', *, *, #4248, .T. ) ;
#753 = CYLINDRICAL_SURFACE ( 'NONE', #10833, 0.06000000000000001860 ) ;
#754 = VERTEX_POINT ( 'NONE', #12861 ) ;
#755 = DIRECTION ( 'NONE',  ( -1.000000000000000000, -0.000000000000000000, -0.000000000000000000 ) ) ;
#756 = DIRECTION ( 'NONE',  ( 0.000000000000000000, 0.000000000000000000, 1.000000000000000000 ) ) ;
#757 = AXIS2_PLACEMENT_3D ( 'NONE', #6640, #6711, #10307 ) ;
#758 = CARTESIAN_POINT ( 'NONE',  ( 1.000048944713735732, -0.4428998280398803722, -0.4293350073753850471 ) ) ;
#759 = ORIENTED_EDGE ( 'NONE', *, *, #973, .F. ) ;
#760 = DIRECTION ( 'NONE',  ( 0.000000000000000000, 1.000000000000000000, 0.000000000000000000 ) ) ;
#761 = LINE ( 'NONE', #7984, #1027 ) ;
#762 = DIRECTION ( 'NONE',  ( 0.000000000000000000, 0.000000000000000000, 1.000000000000000000 ) ) ;
#763 = ORIENTED_EDGE ( 'NONE', *, *, #3098, .T. ) ;
#764 = ORIENTED_EDGE ( 'NONE', *, *, #13005, .T. ) ;
#765 = CIRCLE ( 'NONE', #14467, 1.000000000000000000 ) ;
#766 = DIRECTION ( 'NONE',  ( -0.000000000000000000, 1.000000000000000000, -0.000000000000000000 ) ) ;
#767 = ORIENTED_EDGE ( 'NONE', *, *, #10111, .T. ) ;
#768 = DIRECTION ( 'NONE',  ( -1.000000000000000000, -0.000000000000000000, -0.000000000000000000 ) ) ;
#769 = CARTESIAN_POINT ( 'NONE',  ( 0.6583850202313374922, -0.3799842706883578280, -0.5137832895838266856 ) ) ;
#770 = PRODUCT_DEFINITION_SHAPE ( 'NONE', 'NONE',  #6322 ) ;
#771 = AXIS2_PLACEMENT_3D ( 'NONE', #2349, #11688, #5650 ) ;
#772 = CARTESIAN_POINT ( 'NONE',  ( 0.8999999999999999112, -0.4429999999999998939, -0.3750000000000000555 ) ) ;
#773 = VECTOR ( 'NONE', #11928, 39.37007874015748143 ) ;
#774 = DIRECTION ( 'NONE',  ( 0.000000000000000000, 0.000000000000000000, -1.000000000000000000 ) ) ;
#775 = EDGE_CURVE ( 'NONE', #8481, #1001, #765, .T. ) ;
#776 = AXIS2_PLACEMENT_3D ( 'NONE', #12632, #5620, #13700 ) ;
#777 = EDGE_LOOP ( 'NONE', ( #9479, #72, #11887, #9960 ) ) ;
#778 = ADVANCED_FACE ( 'NONE', ( #1231 ), #10577, .F. ) ;
#779 = CARTESIAN_POINT ( 'NONE',  ( 4.147377230984255370, 1.742726334417983081, -0.7003979466013926514 ) ) ;
#780 = EDGE_LOOP ( 'NONE', ( #12883, #10333, #9108, #10071 ) ) ;
#781 = ORIENTED_EDGE ( 'NONE', *, *, #14687, .T. ) ;
#782 = ADVANCED_FACE ( 'NONE', ( #13010 ), #2472, .F. ) ;
#783 = ORIENTED_EDGE ( 'NONE', *, *, #3012, .F. ) ;
#784 = DIRECTION ( 'NONE',  ( -0.000000000000000000, -1.000000000000000000, -0.000000000000000000 ) ) ;
#785 = CARTESIAN_POINT ( 'NONE',  ( 0.8999999999999999112, -0.4829999999999998739, -0.3750000000000000555 ) ) ;
#786 = DIRECTION ( 'NONE',  ( -0.000000000000000000, -1.000000000000000000, -0.000000000000000000 ) ) ;
#787 = CARTESIAN_POINT ( 'NONE',  ( 0.03634916050344778882, 1.602949386431022472, -0.3809527529760087239 ) ) ;
#788 = VERTEX_POINT ( 'NONE', #6918 ) ;
#789 = LINE ( 'NONE', #5486, #7557 ) ;
#790 = CARTESIAN_POINT ( 'NONE',  ( 3.602264755523620465, 0.9969999999999996643, -0.4491205543005138412 ) ) ;
#791 = AXIS2_PLACEMENT_3D ( 'NONE', #1531, #10950, #4998 ) ;
#792 = DIRECTION ( 'NONE',  ( -0.01412288512831583534, 0.000000000000000000, 0.9999002670844989726 ) ) ;
#793 = EDGE_CURVE ( 'NONE', #6575, #12377, #7154, .T. ) ;
#794 = AXIS2_PLACEMENT_3D ( 'NONE', #10044, #678, #9045 ) ;
#795 = ADVANCED_FACE ( 'NONE', ( #11574 ), #1074, .T. ) ;
#796 = CYLINDRICAL_SURFACE ( 'NONE', #10578, 0.7500000000000001110 ) ;
#797 = CARTESIAN_POINT ( 'NONE',  ( 4.574008775633079615, 1.717466915705979646, 0.4004807778818798014 ) ) ;
#799 = VERTEX_POINT ( 'NONE', #14529 ) ;
#798 = DIRECTION ( 'NONE',  ( 0.000000000000000000, 0.000000000000000000, -1.000000000000000000 ) ) ;
#800 = ADVANCED_FACE ( 'NONE', ( #6370 ), #12022, .T. ) ;
#801 = VERTEX_POINT ( 'NONE', #11094 ) ;
#803 = VERTEX_POINT ( 'NONE', #9804 ) ;
#802 = LINE ( 'NONE', #5576, #10673 ) ;
#804 = ORIENTED_EDGE ( 'NONE', *, *, #3082, .T. ) ;
#805 = EDGE_CURVE ( 'NONE', #9005, #8364, #589, .T. ) ;
#806 = DIRECTION ( 'NONE',  ( 0.000000000000000000, 0.000000000000000000, -1.000000000000000000 ) ) ;
#807 =( NAMED_UNIT ( * ) PLANE_ANGLE_UNIT ( ) SI_UNIT ( $, .RADIAN. ) );
#808 = CARTESIAN_POINT ( 'NONE',  ( -0.4125000000000001998, -0.6290000000000005587, -0.4125000000000000333 ) ) ;
#809 = ORIENTED_EDGE ( 'NONE', *, *, #11407, .T. ) ;
#810 = DIRECTION ( 'NONE',  ( 0.000000000000000000, 0.000000000000000000, -1.000000000000000000 ) ) ;
#811 = CARTESIAN_POINT ( 'NONE',  ( -0.4349147617188414694, 0.7512260236060024354, -0.008611041693271251005 ) ) ;
#812 = B_SPLINE_CURVE_WITH_KNOTS ( 'NONE', 3,
 ( #9229, #13867, #12153, #1661, #5194, #4045, #7170, #3565, #8088, #11824, #14025, #10448, #13028, #5868 ),
 .UNSPECIFIED., .F., .F.,
 ( 4, 2, 2, 2, 2, 2, 4 ),
 ( 0.000000000000000000, 0.0009187753074270573741, 0.001837550614854114748, 0.002296938268567648260, 0.002756325922281181989, 0.003215713575994715284, 0.003675101229708249012 ),
 .UNSPECIFIED. ) ;
#813 = DIRECTION ( 'NONE',  ( 0.000000000000000000, 0.000000000000000000, -1.000000000000000000 ) ) ;
#814 = CARTESIAN_POINT ( 'NONE',  ( 0.09500000000000431710, 1.679378605318059492, 1.304378605318041062 ) ) ;
#815 = AXIS2_PLACEMENT_3D ( 'NONE', #568, #5264, #276 ) ;
#816 = DIRECTION ( 'NONE',  ( 0.000000000000000000, 0.000000000000000000, -1.000000000000000000 ) ) ;
#817 = PRODUCT_DEFINITION_FORMATION_WITH_SPECIFIED_SOURCE ( 'ANY', '', #5185, .NOT_KNOWN. ) ;
#818 = EDGE_LOOP ( 'NONE', ( #5751, #3194 ) ) ;
#819 = DIRECTION ( 'NONE',  ( 0.3420201433256620516, 0.000000000000000000, 0.9396926207859108704 ) ) ;
#820 = CARTESIAN_POINT ( 'NONE',  ( 1.000000000000000222, -0.4429999999999998939, -0.3182109165419975683 ) ) ;
#821 = CARTESIAN_POINT ( 'NONE',  ( 3.874999999999999556, 3.567999999999999616, -1.820000000000000284 ) ) ;
#822 = EDGE_CURVE ( 'NONE', #4210, #2008, #1602, .T. ) ;
#823 = CARTESIAN_POINT ( 'NONE',  ( 0.7038870757886628304, -0.3873557849635640427, 0.4900580921498779996 ) ) ;
#824 = CARTESIAN_POINT ( 'NONE',  ( 6.794491571325179891, 1.679378605318035733, -1.679378605318065487 ) ) ;
#825 = ORIENTED_EDGE ( 'NONE', *, *, #7407, .T. ) ;
#826 = AXIS2_PLACEMENT_3D ( 'NONE', #13633, #4090, #13553 ) ;
#827 = CYLINDRICAL_SURFACE ( 'NONE', #7196, 0.3750000000000007772 ) ;
#828 = ORIENTED_EDGE ( 'NONE', *, *, #12802, .F. ) ;
#829 = CARTESIAN_POINT ( 'NONE',  ( -5.764454660286586870E-18, 0.1759999999999999065, 0.000000000000000000 ) ) ;
#830 = CIRCLE ( 'NONE', #584, 0.9999999999999996669 ) ;
#831 = EDGE_CURVE ( 'NONE', #947, #3137, #10571, .T. ) ;
#832 = DIRECTION ( 'NONE',  ( 0.000000000000000000, 0.000000000000000000, -1.000000000000000000 ) ) ;
#833 = LINE ( 'NONE', #11567, #4529 ) ;
#834 = DIRECTION ( 'NONE',  ( 0.000000000000000000, 0.000000000000000000, -1.000000000000000000 ) ) ;
#835 = ORIENTED_EDGE ( 'NONE', *, *, #7606, .T. ) ;
#836 = CIRCLE ( 'NONE', #13302, 0.4349999999999999423 ) ;
#837 = CARTESIAN_POINT ( 'NONE',  ( 0.4425000000000002820, 0.2159999999999999420, -0.3725000000000000533 ) ) ;
#838 = CARTESIAN_POINT ( 'NONE',  ( 0.8337700833007937185, -0.4835922659884503982, -0.3396222324529075687 ) ) ;
#839 = CIRCLE ( 'NONE', #10405, 0.4070000000000058016 ) ;
#840 = VECTOR ( 'NONE', #1217, 39.37007874015748143 ) ;
#841 = DIRECTION ( 'NONE',  ( 1.000000000000000000, 0.000000000000000000, 0.000000000000000000 ) ) ;
#842 = CARTESIAN_POINT ( 'NONE',  ( 0.7371172985291584157, -0.4420715194279608018, -0.4420151072446013574 ) ) ;
#843 = VERTEX_POINT ( 'NONE', #2922 ) ;
#844 = ORIENTED_EDGE ( 'NONE', *, *, #11893, .T. ) ;
#845 = CYLINDRICAL_SURFACE ( 'NONE', #14549, 0.2624999999999994560 ) ;
#846 = ORIENTED_EDGE ( 'NONE', *, *, #5437, .T. ) ;
#847 = DIRECTION ( 'NONE',  ( 1.000000000000000000, 0.000000000000000000, 0.000000000000000000 ) ) ;
#848 = CARTESIAN_POINT ( 'NONE',  ( 0.6773748815706881476, -0.3764079396444222625, -0.4904325581699054970 ) ) ;
#849 = EDGE_CURVE ( 'NONE', #7678, #799, #9607, .T. ) ;
#850 = AXIS2_PLACEMENT_3D ( 'NONE', #3235, #7900, #12551 ) ;
#851 = FACE_OUTER_BOUND ( 'NONE', #20, .T. ) ;
#852 = CIRCLE ( 'NONE', #6252, 0.4999999999999995004 ) ;
#853 = CONICAL_SURFACE ( 'NONE', #14058, 0.07000000000000047851, 0.7853981633974297383 ) ;
#854 = DIRECTION ( 'NONE',  ( 1.000000000000000000, 0.000000000000000000, 0.000000000000000000 ) ) ;
#855 = ORIENTED_EDGE ( 'NONE', *, *, #6620, .T. ) ;
#856 = DIRECTION ( 'NONE',  ( 0.000000000000000000, 0.000000000000000000, 1.000000000000000000 ) ) ;
#857 = CIRCLE ( 'NONE', #5772, 0.2624999999999852451 ) ;
#858 = ORIENTED_EDGE ( 'NONE', *, *, #6303, .T. ) ;
#859 = CIRCLE ( 'NONE', #6268, 2.967999999999998639 ) ;
#860 = ORIENTED_EDGE ( 'NONE', *, *, #4113, .T. ) ;
#861 = CIRCLE ( 'NONE', #4805, 0.4999999999999997224 ) ;
#862 = PLANE ( 'NONE',  #8468 ) ;
#863 = VERTEX_POINT ( 'NONE', #1533 ) ;
#864 = CARTESIAN_POINT ( 'NONE',  ( 0.4108223460329283871, 5.750000000000000000, 0.2850000000000014189 ) ) ;
#865 = DIRECTION ( 'NONE',  ( -0.000000000000000000, -1.000000000000000000, -0.000000000000000000 ) ) ;
#866 = FACE_OUTER_BOUND ( 'NONE', #10958, .T. ) ;
#867 = CARTESIAN_POINT ( 'NONE',  ( -0.1444275314249775788, 1.589819979576904130, 0.3809527529760086684 ) ) ;
#868 = ORIENTED_EDGE ( 'NONE', *, *, #6140, .T. ) ;
#869 = PRODUCT_DEFINITION ( 'UNKNOWN', '', #12798, #3254 ) ;
#870 = CARTESIAN_POINT ( 'NONE',  ( 3.319143374005773861, 2.449058936906570061, -0.5026158830344926720 ) ) ;
#871 = VECTOR ( 'NONE', #15054, 39.37007874015748143 ) ;
#872 = SURFACE_SIDE_STYLE ('',( #14669 ) ) ;
#873 = CIRCLE ( 'NONE', #14568, 0.2432499999999999385 ) ;
#874 = FACE_OUTER_BOUND ( 'NONE', #12768, .T. ) ;
#875 = CYLINDRICAL_SURFACE ( 'NONE', #13931, 0.2624999999999852451 ) ;
#876 = CARTESIAN_POINT ( 'NONE',  ( 4.465766375128255916, 1.731456125583728634, 0.4644050319404698368 ) ) ;
#878 = ORIENTED_EDGE ( 'NONE', *, *, #13318, .T. ) ;
#877 = DIRECTION ( 'NONE',  ( 0.000000000000000000, 0.000000000000000000, 1.000000000000000000 ) ) ;
#879 = AXIS2_PLACEMENT_3D ( 'NONE', #13795, #13568, #5559 ) ;
#880 = ORIENTED_EDGE ( 'NONE', *, *, #3562, .T. ) ;
#882 = ORIENTED_EDGE ( 'NONE', *, *, #10381, .T. ) ;
#881 = FACE_OUTER_BOUND ( 'NONE', #11882, .T. ) ;
#883 = ORIENTED_EDGE ( 'NONE', *, *, #8087, .F. ) ;
#884 = ADVANCED_FACE ( 'NONE', ( #7508 ), #10805, .T. ) ;
#885 = EDGE_CURVE ( 'NONE', #1422, #2642, #6660, .T. ) ;
#886 = CARTESIAN_POINT ( 'NONE',  ( 0.000000000000000000, 1.109999999999999876, 0.000000000000000000 ) ) ;
#887 = DIRECTION ( 'NONE',  ( 0.000000000000000000, 0.000000000000000000, -1.000000000000000000 ) ) ;
#888 = ORIENTED_EDGE ( 'NONE', *, *, #2012, .T. ) ;
#889 = EDGE_CURVE ( 'NONE', #5675, #3668, #5000, .T. ) ;
#890 = CARTESIAN_POINT ( 'NONE',  ( 2.774999999999999911, -0.9799999999999436939, 3.360000000000016751 ) ) ;
#891 = LINE ( 'NONE', #9338, #9977 ) ;
#892 = VECTOR ( 'NONE', #8627, 39.37007874015748143 ) ;
#893 = CARTESIAN_POINT ( 'NONE',  ( 3.921039573451326365, 1.873037145645487955, 0.4984214080510448452 ) ) ;
#894 = DIRECTION ( 'NONE',  ( 1.000000000000000000, 0.000000000000000000, 0.000000000000000000 ) ) ;
#895 = EDGE_CURVE ( 'NONE', #15127, #2763, #9957, .T. ) ;
#896 = EDGE_CURVE ( 'NONE', #6953, #3491, #7435, .T. ) ;
#897 = CARTESIAN_POINT ( 'NONE',  ( 2.381934877626368241, 0.6476033094205475571, -0.4663568520109309112 ) ) ;
#898 = CARTESIAN_POINT ( 'NONE',  ( 3.601417382415921686, 1.056999999999999718, -0.3891265382754440227 ) ) ;
#899 = ORIENTED_EDGE ( 'NONE', *, *, #1393, .F. ) ;
#900 = CARTESIAN_POINT ( 'NONE',  ( 2.156999999999999584, 1.679378605318042395, -1.679378605318058604 ) ) ;
#901 = CARTESIAN_POINT ( 'NONE',  ( 2.743000000000000771, 1.679378605318059048, 1.679378605318041506 ) ) ;
#902 = CIRCLE ( 'NONE', #7517, 0.1068000000000000754 ) ;
#903 = DIRECTION ( 'NONE',  ( 0.000000000000000000, 0.000000000000000000, -1.000000000000000000 ) ) ;
#904 = DIRECTION ( 'NONE',  ( -1.000000000000000000, 0.000000000000000000, -1.047444401652940007E-14 ) ) ;
#906 = VERTEX_POINT ( 'NONE', #7299 ) ;
#905 = CARTESIAN_POINT ( 'NONE',  ( 2.774999999999999911, -0.9799999999999436939, 2.360000000000016307 ) ) ;
#907 = ORIENTED_EDGE ( 'NONE', *, *, #14977, .T. ) ;
#908 = FACE_OUTER_BOUND ( 'NONE', #13181, .T. ) ;
#909 = VERTEX_POINT ( 'NONE', #13161 ) ;
#910 = DIRECTION ( 'NONE',  ( -1.000000000000000000, -1.689854595570744117E-16, 0.000000000000000000 ) ) ;
#911 = VECTOR ( 'NONE', #11865, 39.37007874015748143 ) ;
#912 = DIRECTION ( 'NONE',  ( -0.000000000000000000, -1.000000000000000000, -0.000000000000000000 ) ) ;
#913 = DIRECTION ( 'NONE',  ( 0.000000000000000000, 0.000000000000000000, 1.000000000000000000 ) ) ;
#914 = CIRCLE ( 'NONE', #14855, 0.05999999999999994227 ) ;
#915 = DIRECTION ( 'NONE',  ( 0.000000000000000000, 0.000000000000000000, -1.000000000000000000 ) ) ;
#916 = EDGE_CURVE ( 'NONE', #14996, #14785, #11953, .T. ) ;
#917 = AXIS2_PLACEMENT_3D ( 'NONE', #9344, #10631, #8199 ) ;
#918 = ORIENTED_EDGE ( 'NONE', *, *, #7315, .T. ) ;
#919 = CARTESIAN_POINT ( 'NONE',  ( 6.096491571325181269, 1.836970198721030181E-16, -1.500000000000000222 ) ) ;
#920 = CARTESIAN_POINT ( 'NONE',  ( 0.8418300605894719624, -0.4829999999999998739, -0.3276580719765713745 ) ) ;
#921 = CIRCLE ( 'NONE', #11927, 0.5000000000000000000 ) ;
#922 = ADVANCED_FACE ( 'NONE', ( #1460 ), #7370, .F. ) ;
#923 = FACE_OUTER_BOUND ( 'NONE', #1949, .T. ) ;
#924 = ORIENTED_EDGE ( 'NONE', *, *, #3817, .T. ) ;
#925 = CARTESIAN_POINT ( 'NONE',  ( 0.1807106342563528367, 1.379999999999999671, 5.178337979384803075E-18 ) ) ;
#926 = DIRECTION ( 'NONE',  ( 0.000000000000000000, -0.7071067811865501263, -0.7071067811865449082 ) ) ;
#927 = CARTESIAN_POINT ( 'NONE',  ( 1.250847373107698779, -0.05999999999999997696, 0.4823326642216426707 ) ) ;
#928 = ORIENTED_EDGE ( 'NONE', *, *, #147, .T. ) ;
#929 = CARTESIAN_POINT ( 'NONE',  ( 0.09035531712817648775, 1.629999999999999893, -0.1564999999999998892 ) ) ;
#930 = AXIS2_PLACEMENT_3D ( 'NONE', #1529, #367, #7504 ) ;
#931 = VECTOR ( 'NONE', #1357, 39.37007874015748143 ) ;
#932 = DIRECTION ( 'NONE',  ( -0.000000000000000000, -1.000000000000000000, -0.000000000000000000 ) ) ;
#933 = AXIS2_PLACEMENT_3D ( 'NONE', #295, #6071, #11651 ) ;
#934 = DIRECTION ( 'NONE',  ( 1.000000000000000000, 0.000000000000000000, 0.000000000000000000 ) ) ;
#935 = CIRCLE ( 'NONE', #7791, 1.580000000000000071 ) ;
#936 = CARTESIAN_POINT ( 'NONE',  ( 4.113165067732116320, 1.797094705958242722, -0.7133961233632938326 ) ) ;
#937 = VERTEX_POINT ( 'NONE', #5073 ) ;
#938 = CARTESIAN_POINT ( 'NONE',  ( -0.4108223460329323840, 4.529999999999999361, 0.2849999999999956457 ) ) ;
#939 = ADVANCED_FACE ( 'NONE', ( #447 ), #5148, .T. ) ;
#940 = EDGE_CURVE ( 'NONE', #5002, #12407, #1270, .T. ) ;
#941 = CARTESIAN_POINT ( 'NONE',  ( 3.589981441049234334, 1.905209480108689402, -0.6943159375963412483 ) ) ;
#942 = ORIENTED_EDGE ( 'NONE', *, *, #7538, .T. ) ;
#943 = ORIENTED_EDGE ( 'NONE', *, *, #13912, .T. ) ;
#944 = AXIS2_PLACEMENT_3D ( 'NONE', #1331, #3727, #7024 ) ;
#945 = UNCERTAINTY_MEASURE_WITH_UNIT (LENGTH_MEASURE( 1.000000000000000082E-05 ), #5734, 'distance_accuracy_value', 'NONE');
#946 = FACE_OUTER_BOUND ( 'NONE', #13192, .T. ) ;
#947 = VERTEX_POINT ( 'NONE', #9877 ) ;
#948 = LINE ( 'NONE', #12355, #2616 ) ;
#949 = CARTESIAN_POINT ( 'NONE',  ( 0.000000000000000000, 0.000000000000000000, 0.000000000000000000 ) ) ;
#950 = DIRECTION ( 'NONE',  ( 0.7070715176384863021, 0.7070715176384774203, 0.009986885842351498482 ) ) ;
#951 = CARTESIAN_POINT ( 'NONE',  ( 0.07259084472369427277, 1.600827197418697168, -0.3809527529760087794 ) ) ;
#952 = EDGE_LOOP ( 'NONE', ( #12292, #10995, #9837, #7098 ) ) ;
#953 = DIRECTION ( 'NONE',  ( 0.000000000000000000, 0.000000000000000000, -1.000000000000000000 ) ) ;
#954 = CARTESIAN_POINT ( 'NONE',  ( 6.826491571325181695, 1.679378605318059492, 2.054378605318042172 ) ) ;
#955 = DIRECTION ( 'NONE',  ( 0.000000000000000000, 0.000000000000000000, -1.000000000000000000 ) ) ;
#956 = CIRCLE ( 'NONE', #10758, 0.5000000000000000000 ) ;
#957 = CARTESIAN_POINT ( 'NONE',  ( 0.000000000000000000, 0.000000000000000000, 0.000000000000000000 ) ) ;
#958 = EDGE_CURVE ( 'NONE', #7795, #14642, #9107, .T. ) ;
#959 = CARTESIAN_POINT ( 'NONE',  ( 4.552750260792047143, 1.739117664213755576, -0.3249664550261794349 ) ) ;
#961 = ORIENTED_EDGE ( 'NONE', *, *, #6008, .F. ) ;
#960 = LINE ( 'NONE', #2031, #6707 ) ;
#962 = ORIENTED_EDGE ( 'NONE', *, *, #7688, .F. ) ;
#964 = ORIENTED_EDGE ( 'NONE', *, *, #2726, .T. ) ;
#963 = CARTESIAN_POINT ( 'NONE',  ( 3.211636230763933762E-17, 1.629999999999999893, 0.2432499999999999385 ) ) ;
#965 = ORIENTED_EDGE ( 'NONE', *, *, #1473, .F. ) ;
#966 = DIRECTION ( 'NONE',  ( -0.000000000000000000, -1.000000000000000000, -0.000000000000000000 ) ) ;
#967 = CARTESIAN_POINT ( 'NONE',  ( 0.000000000000000000, 0.000000000000000000, 0.000000000000000000 ) ) ;
#968 = DIRECTION ( 'NONE',  ( -1.000000000000000000, -0.000000000000000000, -0.000000000000000000 ) ) ;
#969 = VERTEX_POINT ( 'NONE', #13683 ) ;
#970 = DIRECTION ( 'NONE',  ( -0.000000000000000000, -1.000000000000000000, -0.000000000000000000 ) ) ;
#971 = DIRECTION ( 'NONE',  ( -1.000000000000000000, -0.000000000000000000, -0.000000000000000000 ) ) ;
#972 = DIRECTION ( 'NONE',  ( -0.000000000000000000, -1.000000000000000000, 0.000000000000000000 ) ) ;
#973 = EDGE_CURVE ( 'NONE', #6575, #638, #4002, .T. ) ;
#974 = CARTESIAN_POINT ( 'NONE',  ( -0.7287617923574203349, -0.6590000000000000302, -0.4424999999999983391 ) ) ;
#975 = EDGE_CURVE ( 'NONE', #9328, #8969, #4295, .T. ) ;
#976 = FACE_OUTER_BOUND ( 'NONE', #152, .T. ) ;
#977 = EDGE_CURVE ( 'NONE', #8165, #803, #10109, .T. ) ;
#978 = DIRECTION ( 'NONE',  ( 0.000000000000000000, 1.000000000000000000, -0.000000000000000000 ) ) ;
#979 = CARTESIAN_POINT ( 'NONE',  ( 3.499444649685982789, 0.9439035327204450265, -0.3304825201858028749 ) ) ;
#980 = CARTESIAN_POINT ( 'NONE',  ( 3.464708039267614836, 1.935623382077672705, -0.7069089347666170919 ) ) ;
#981 = CARTESIAN_POINT ( 'NONE',  ( 2.774999999999999911, 0.000000000000000000, 0.000000000000000000 ) ) ;
#983 = ORIENTED_EDGE ( 'NONE', *, *, #13062, .T. ) ;
#982 = LINE ( 'NONE', #14995, #3083 ) ;
#984 = EDGE_LOOP ( 'NONE', ( #552, #6719 ) ) ;
#985 = EDGE_CURVE ( 'NONE', #1935, #6943, #14966, .T. ) ;
#986 = FACE_OUTER_BOUND ( 'NONE', #13920, .T. ) ;
#987 = ORIENTED_EDGE ( 'NONE', *, *, #10256, .T. ) ;
#988 = AXIS2_PLACEMENT_3D ( 'NONE', #2346, #31, #11758 ) ;
#989 = LINE ( 'NONE', #9433, #5615 ) ;
#990 = CARTESIAN_POINT ( 'NONE',  ( 2.824624536279081610, 0.5882431044538637410, -0.4601041732163972386 ) ) ;
#991 =( BOUNDED_SURFACE ( )  B_SPLINE_SURFACE ( 3, 2, ( 
 ( #3476, #8235, #2403 ),
 ( #7008, #10589, #2631 ),
 ( #8384, #7089, #14 ),
 ( #11964, #4704, #1316 ),
 ( #6003, #8153, #4936 ),
 ( #11745, #5773, #9455 ),
 ( #8318, #10437, #13097 ),
 ( #13020, #1163, #15097 ),
 ( #10667, #11662, #2482 ),
 ( #4861, #1240, #5859 ) ),
 .UNSPECIFIED., .F., .F., .T. ) 
 B_SPLINE_SURFACE_WITH_KNOTS ( ( 4, 2, 2, 2, 4 ),
 ( 3, 3 ),
 ( 3.926990816987246280, 4.123340357836607240, 4.319689898685967755, 4.516039439535328270, 4.712388980384689674 ),
 ( 0.000000000000000000, 1.000000000000000000 ),
 .UNSPECIFIED. ) 
 GEOMETRIC_REPRESENTATION_ITEM ( )  RATIONAL_B_SPLINE_SURFACE ( (
 ( 1.000000000000000000, 0.7106287314217404338, 1.000000000000000000),
 ( 1.000000000000000000, 0.7103988163329607586, 1.000000000000000000),
 ( 1.000000000000000000, 0.7101460984486431816, 1.000000000000000000),
 ( 1.000000000000000000, 0.7096047632039514941, 1.000000000000000000),
 ( 1.000000000000000000, 0.7093161336535294126, 1.000000000000000000),
 ( 1.000000000000000000, 0.7087139042199988026, 1.000000000000000000),
 ( 1.000000000000000000, 0.7084003186178147171, 1.000000000000000000),
 ( 1.000000000000000000, 0.7077601512495510505, 1.000000000000000000),
 ( 1.000000000000000000, 0.7074335897358576819, 1.000000000000000000),
 ( 1.000000000000000000, 0.7071067811865475727, 1.000000000000000000) ) ) 
 REPRESENTATION_ITEM ( '' )  SURFACE ( )  );
#992 = AXIS2_PLACEMENT_3D ( 'NONE', #11456, #4574, #6795 ) ;
#993 = CARTESIAN_POINT ( 'NONE',  ( 3.394491571325183088, -1.679378605318041950, 1.679378605318059048 ) ) ;
#994 = CARTESIAN_POINT ( 'NONE',  ( 2.774999999999999911, -2.360000000000016751, -0.9799999999999431388 ) ) ;
#995 = EDGE_CURVE ( 'NONE', #11613, #10962, #8387, .T. ) ;
#996 = DIRECTION ( 'NONE',  ( 1.000000000000000000, 0.000000000000000000, 0.000000000000000000 ) ) ;
#997 = EDGE_LOOP ( 'NONE', ( #8693, #7422, #5563, #6768 ) ) ;
#998 = CARTESIAN_POINT ( 'NONE',  ( 0.4124999999999997558, -0.6290000000000003366, -0.4125000000000000333 ) ) ;
#999 = CONICAL_SURFACE ( 'NONE', #1723, 0.2624999999999852451, 0.7853981633974423948 ) ;
#1000 = FACE_OUTER_BOUND ( 'NONE', #10425, .T. ) ;
#1001 = VERTEX_POINT ( 'NONE', #4150 ) ;
#1002 = CARTESIAN_POINT ( 'NONE',  ( 5.567023771132172172, 1.836970198721030181E-16, -1.500000000000000222 ) ) ;
#1003 = ORIENTED_EDGE ( 'NONE', *, *, #4844, .T. ) ;
#1004 = CARTESIAN_POINT ( 'NONE',  ( 8.476283996537762988, 0.8689495495877206377, -0.3203020658980470503 ) ) ;
#1005 = VERTEX_POINT ( 'NONE', #820 ) ;
#1006 = DIRECTION ( 'NONE',  ( 1.000000000000000000, 0.000000000000000000, 0.000000000000000000 ) ) ;
#1007 = EDGE_CURVE ( 'NONE', #11436, #2506, #11250, .T. ) ;
#1008 = CARTESIAN_POINT ( 'NONE',  ( 3.426491571325181340, 2.360000000000015863, 0.9799999999999454703 ) ) ;
#1009 = CIRCLE ( 'NONE', #13710, 0.05999999999999994227 ) ;
#1010 = CARTESIAN_POINT ( 'NONE',  ( 0.8533815140473888228, -0.4340691947652905447, -0.4596148562493023171 ) ) ;
#1011 = EDGE_CURVE ( 'NONE', #3810, #12377, #7828, .T. ) ;
#1012 = CARTESIAN_POINT ( 'NONE',  ( 3.971366415850335230, 1.827788509831742347, -0.7443691409044070895 ) ) ;
#1013 = CARTESIAN_POINT ( 'NONE',  ( 8.783907589752271150, 0.8796920021765856079, 0.08309344507351693054 ) ) ;
#1014 = SHAPE_REPRESENTATION ( 'Handle', ( #8424 ), #9874 ) ;
#1015 = CARTESIAN_POINT ( 'NONE',  ( 3.876040592281544850, 1.779390558749738060, -0.7983410256676741756 ) ) ;
#1016 = EDGE_LOOP ( 'NONE', ( #4083, #3866 ) ) ;
#1017 = VERTEX_POINT ( 'NONE', #3681 ) ;
#1018 = DIRECTION ( 'NONE',  ( 0.000000000000000000, 0.000000000000000000, 1.000000000000000000 ) ) ;
#1019 = ORIENTED_EDGE ( 'NONE', *, *, #8402, .F. ) ;
#1020 = CARTESIAN_POINT ( 'NONE',  ( 3.874999999999999556, 3.137999999999999901, 1.509999999999999787 ) ) ;
#1021 = CARTESIAN_POINT ( 'NONE',  ( 0.2249147617188453907, 1.559103846021540951, 0.3723417112827335784 ) ) ;
#1022 = CARTESIAN_POINT ( 'NONE',  ( 0.09500000000000431710, 1.679378605318059492, 1.679378605318041506 ) ) ;
#1023 = CARTESIAN_POINT ( 'NONE',  ( 2.088768908813758873, 0.2870784642939425146, 0.4704976142822915319 ) ) ;
#1024 = VERTEX_POINT ( 'NONE', #1134 ) ;
#1025 = CARTESIAN_POINT ( 'NONE',  ( -0.3725000000000002198, -0.6590000000000000302, -0.4424999999999983391 ) ) ;
#1026 = EDGE_CURVE ( 'NONE', #11415, #1104, #8866, .T. ) ;
#1027 = VECTOR ( 'NONE', #3234, 39.37007874015748143 ) ;
#1028 = EDGE_CURVE ( 'NONE', #539, #5425, #10488, .T. ) ;
#1029 = EDGE_CURVE ( 'NONE', #10024, #11969, #3447, .T. ) ;
#1030 = CARTESIAN_POINT ( 'NONE',  ( 0.4349147617188415249, 1.239999999999999991, 0.008611041693268213504 ) ) ;
#1031 = LINE ( 'NONE', #4884, #2952 ) ;
#1032 = FILL_AREA_STYLE_COLOUR ( '', #7177 ) ;
#1033 = CARTESIAN_POINT ( 'NONE',  ( 4.527597100494972437, 1.736431947037383683, -0.3728085656124198732 ) ) ;
#1034 = ORIENTED_EDGE ( 'NONE', *, *, #7995, .F. ) ;
#1036 = EDGE_LOOP ( 'NONE', ( #10242, #8055, #6195, #14488, #8462, #4157, #8619, #12945 ) ) ;
#1035 = DIRECTION ( 'NONE',  ( 0.000000000000000000, 0.000000000000000000, 1.000000000000000000 ) ) ;
#1037 = VERTEX_POINT ( 'NONE', #4597 ) ;
#1039 = EDGE_LOOP ( 'NONE', ( #10566, #2298 ) ) ;
#1038 = CARTESIAN_POINT ( 'NONE',  ( 3.874999999999999556, 3.170500000000001428, -1.130000000000000560 ) ) ;
#1040 = VERTEX_POINT ( 'NONE', #7133 ) ;
#1041 = CARTESIAN_POINT ( 'NONE',  ( 4.344846310392954436, 3.567999999999999616, 1.491010071662831393 ) ) ;
#1042 = DIRECTION ( 'NONE',  ( 1.000000000000000000, 0.000000000000000000, 0.000000000000000000 ) ) ;
#1043 = VERTEX_POINT ( 'NONE', #2216 ) ;
#1044 = VECTOR ( 'NONE', #4168, 39.37007874015748143 ) ;
#1045 = CARTESIAN_POINT ( 'NONE',  ( 6.215861650065340527, 3.673940397442060361E-16, 3.000000000000000444 ) ) ;
#1046 = CARTESIAN_POINT ( 'NONE',  ( 0.7017867892446607581, -0.4844395604395603239, -0.4010711782184315233 ) ) ;
#1047 = AXIS2_PLACEMENT_3D ( 'NONE', #11257, #6751, #598 ) ;
#1048 = ADVANCED_FACE ( 'NONE', ( #12992, #4746 ), #10329, .F. ) ;
#1049 = DIRECTION ( 'NONE',  ( 0.000000000000000000, 0.000000000000000000, 1.000000000000000000 ) ) ;
#1050 = CARTESIAN_POINT ( 'NONE',  ( 3.601417382415921686, -0.9430000000000002824, 0.5000000000000000000 ) ) ;
#1051 = ADVANCED_FACE ( 'NONE', ( #9272 ), #11784, .F. ) ;
#1052 = CARTESIAN_POINT ( 'NONE',  ( 2.774999999999999911, 0.000000000000000000, 0.000000000000000000 ) ) ;
#1053 = DIRECTION ( 'NONE',  ( 0.7071067811865471286, 0.000000000000000000, -0.7071067811865479058 ) ) ;
#1054 = CARTESIAN_POINT ( 'NONE',  ( -0.4124999999999999223, 0.000000000000000000, -0.4124999999999999778 ) ) ;
#1055 = AXIS2_PLACEMENT_3D ( 'NONE', #7952, #12603, #6816 ) ;
#1056 = DIRECTION ( 'NONE',  ( 1.874307916738608820E-16, -1.000000000000000000, -0.000000000000000000 ) ) ;
#1057 = CARTESIAN_POINT ( 'NONE',  ( 4.271292041023736274, 1.710010143222131740, 0.6913003412368600165 ) ) ;
#1058 = AXIS2_PLACEMENT_3D ( 'NONE', #7084, #1237, #9450 ) ;
#1059 = CARTESIAN_POINT ( 'NONE',  ( 0.000000000000000000, 4.529999999999999361, 0.000000000000000000 ) ) ;
#1061 = ORIENTED_EDGE ( 'NONE', *, *, #6248, .F. ) ;
#1060 = PLANE ( 'NONE',  #1361 ) ;
#1062 = VERTEX_POINT ( 'NONE', #127 ) ;
#1063 = DIRECTION ( 'NONE',  ( -0.000000000000000000, -1.000000000000000000, -0.000000000000000000 ) ) ;
#1064 = EDGE_LOOP ( 'NONE', ( #12205, #10313, #3455, #7403 ) ) ;
#1065 = EDGE_CURVE ( 'NONE', #5891, #9216, #4828, .T. ) ;
#1066 = CYLINDRICAL_SURFACE ( 'NONE', #5370, 0.5000000000000002220 ) ;
#1067 = CARTESIAN_POINT ( 'NONE',  ( 2.855088541747186515, 0.5369222675350495688, -0.4596738906532820690 ) ) ;
#1068 = AXIS2_PLACEMENT_3D ( 'NONE', #4518, #1981, #6901 ) ;
#1069 = CARTESIAN_POINT ( 'NONE',  ( 2.282850251811598064, 0.09542856769877475220, 0.4677563523755423613 ) ) ;
#1070 = CARTESIAN_POINT ( 'NONE',  ( 2.774999999999999911, -3.360000000000016751, -0.9799999999999434719 ) ) ;
#1071 = DIRECTION ( 'NONE',  ( -2.602462600580852055E-17, -1.000000000000000000, -4.814436796019480615E-35 ) ) ;
#1072 = EDGE_LOOP ( 'NONE', ( #4283, #12804 ) ) ;
#1073 = CARTESIAN_POINT ( 'NONE',  ( 0.7017867892446613132, -0.4844395604395603239, 0.4010711782184302465 ) ) ;
#1074 = CYLINDRICAL_SURFACE ( 'NONE', #2512, 0.5000000000000002220 ) ;
#1075 = ORIENTED_EDGE ( 'NONE', *, *, #4649, .F. ) ;
#1076 = CIRCLE ( 'NONE', #96, 0.2499999999999999167 ) ;
#1077 = FACE_OUTER_BOUND ( 'NONE', #8580, .T. ) ;
#1078 = ORIENTED_EDGE ( 'NONE', *, *, #4120, .F. ) ;
#1079 = DIRECTION ( 'NONE',  ( -1.000000000000000000, -0.000000000000000000, -0.000000000000000000 ) ) ;
#1080 = VERTEX_POINT ( 'NONE', #13983 ) ;
#1081 = EDGE_CURVE ( 'NONE', #3261, #1080, #6900, .T. ) ;
#1082 = DIRECTION ( 'NONE',  ( -1.000000000000000000, -0.000000000000000000, -0.000000000000000000 ) ) ;
#1083 = EDGE_CURVE ( 'NONE', #8323, #8852, #8201, .T. ) ;
#1084 = EDGE_CURVE ( 'NONE', #1606, #10100, #1432, .T. ) ;
#1085 = CARTESIAN_POINT ( 'NONE',  ( 0.09500000000000431710, 1.679378605318059492, 1.304378605318041062 ) ) ;
#1086 = CIRCLE ( 'NONE', #5244, 0.2624999999999852451 ) ;
#1087 = CARTESIAN_POINT ( 'NONE',  ( 3.995454032860411342, 1.821680253208853406, -0.7409104450711488932 ) ) ;
#1088 = CIRCLE ( 'NONE', #5496, 0.03999999999999998002 ) ;
#1089 = VECTOR ( 'NONE', #11315, 39.37007874015748143 ) ;
#1090 = EDGE_CURVE ( 'NONE', #7832, #9046, #9515, .T. ) ;
#1091 = FACE_OUTER_BOUND ( 'NONE', #12888, .T. ) ;
#1092 = CARTESIAN_POINT ( 'NONE',  ( 3.898431109275737771, 1.794535650040266495, -0.7500217376237132694 ) ) ;
#1093 = ORIENTED_EDGE ( 'NONE', *, *, #2010, .T. ) ;
#1094 = ORIENTED_EDGE ( 'NONE', *, *, #4898, .F. ) ;
#1095 = PRODUCT_DEFINITION_CONTEXT ( 'detailed design', #1849, 'design' ) ;
#1096 = AXIS2_PLACEMENT_3D ( 'NONE', #2994, #3927, #523 ) ;
#1097 = DIRECTION ( 'NONE',  ( -0.9992912762382412106, -0.03489602031262427351, 0.01411428356269048105 ) ) ;
#1098 = ORIENTED_EDGE ( 'NONE', *, *, #13912, .F. ) ;
#1099 = CARTESIAN_POINT ( 'NONE',  ( 0.4313007445438669096, 1.564783867144734497, -0.01487070305975950364 ) ) ;
#1100 = CIRCLE ( 'NONE', #6245, 0.2944999999999987073 ) ;
#1101 = CARTESIAN_POINT ( 'NONE',  ( 0.8410094793127153023, -0.4816416392817352565, -0.4218009027733075067 ) ) ;
#1102 = FACE_OUTER_BOUND ( 'NONE', #10925, .T. ) ;
#1103 = CARTESIAN_POINT ( 'NONE',  ( 2.774999999999999911, -1.679378605318041950, 1.384878605318060174 ) ) ;
#1104 = VERTEX_POINT ( 'NONE', #11717 ) ;
#1105 = CARTESIAN_POINT ( 'NONE',  ( 3.263555662057198603, 2.462108353317236986, -0.4359725516674392565 ) ) ;
#1106 = CARTESIAN_POINT ( 'NONE',  ( 0.7026382878071448790, -0.05185562024730498015, -0.4896667335905589558 ) ) ;
#1107 = DIRECTION ( 'NONE',  ( 0.000000000000000000, -1.000000000000000000, 0.000000000000000000 ) ) ;
#1108 = EDGE_CURVE ( 'NONE', #14200, #7033, #1666, .T. ) ;
#1109 = CIRCLE ( 'NONE', #6756, 0.7849999999999983658 ) ;
#1110 = EDGE_CURVE ( 'NONE', #9095, #13586, #9853, .T. ) ;
#1111 = TOROIDAL_SURFACE ( 'NONE', #6254, 0.0001794190581142465670, 1.999999999999999334 ) ;
#1112 = DIRECTION ( 'NONE',  ( 0.000000000000000000, 0.000000000000000000, -1.000000000000000000 ) ) ;
#1113 = CARTESIAN_POINT ( 'NONE',  ( 4.680319326871657637, 1.732346333260918803, -0.09359317111134475564 ) ) ;
#1114 = EDGE_LOOP ( 'NONE', ( #14102, #6669, #12830, #8989 ) ) ;
#1116 = ORIENTED_EDGE ( 'NONE', *, *, #5437, .F. ) ;
#1115 = CARTESIAN_POINT ( 'NONE',  ( 2.774999999999999911, 0.000000000000000000, 0.000000000000000000 ) ) ;
#1117 = EDGE_CURVE ( 'NONE', #2506, #3160, #2903, .T. ) ;
#1118 = ORIENTED_EDGE ( 'NONE', *, *, #3684, .F. ) ;
#1120 = ORIENTED_EDGE ( 'NONE', *, *, #6402, .F. ) ;
#1119 = CARTESIAN_POINT ( 'NONE',  ( 0.09500000000000431710, -1.679378605318047946, -2.054378605318054163 ) ) ;
#1121 = ORIENTED_EDGE ( 'NONE', *, *, #4050, .T. ) ;
#1122 = CARTESIAN_POINT ( 'NONE',  ( 0.09035531712817643224, 1.379999999999999671, 0.1564999999999999447 ) ) ;
#1123 = LENGTH_MEASURE_WITH_UNIT ( LENGTH_MEASURE( 0.02539999999999999897 ), #3281 );
#1124 = DIRECTION ( 'NONE',  ( 0.000000000000000000, 0.000000000000000000, 1.000000000000000000 ) ) ;
#1125 = ORIENTED_EDGE ( 'NONE', *, *, #1582, .F. ) ;
#1126 = CARTESIAN_POINT ( 'NONE',  ( 0.1250000000000009992, 0.000000000000000000, 1.000000000000000000 ) ) ;
#1127 = FACE_OUTER_BOUND ( 'NONE', #1598, .T. ) ;
#1128 = DIRECTION ( 'NONE',  ( 0.01412288512831213171, -3.675428035873183031E-19, 0.9999002670844990837 ) ) ;
#1129 = FACE_OUTER_BOUND ( 'NONE', #9634, .T. ) ;
#1130 = CARTESIAN_POINT ( 'NONE',  ( 0.6179999999999965521, 1.679378605318059492, 1.304378605318041062 ) ) ;
#1131 = LINE ( 'NONE', #974, #3161 ) ;
#1132 = DIRECTION ( 'NONE',  ( 1.000000000000000000, 0.000000000000000000, 0.000000000000000000 ) ) ;
#1133 = DIRECTION ( 'NONE',  ( 0.000000000000000000, 0.000000000000000000, 1.000000000000000000 ) ) ;
#1134 = CARTESIAN_POINT ( 'NONE',  ( 2.045495128834867060, 0.3295048711651353268, 0.4105035982572216025 ) ) ;
#1135 = CARTESIAN_POINT ( 'NONE',  ( 4.660391722812436299, 1.729108088022653922, 0.1957348282867307776 ) ) ;
#1136 = EDGE_CURVE ( 'NONE', #14886, #5214, #8635, .T. ) ;
#1137 = ORIENTED_EDGE ( 'NONE', *, *, #12490, .F. ) ;
#1138 = FACE_OUTER_BOUND ( 'NONE', #7580, .T. ) ;
#1139 = VECTOR ( 'NONE', #5504, 39.37007874015748143 ) ;
#1141 = ORIENTED_EDGE ( 'NONE', *, *, #52, .T. ) ;
#1140 = DIRECTION ( 'NONE',  ( -1.365923996832131609E-16, 1.000000000000000000, -0.000000000000000000 ) ) ;
#1142 = ORIENTED_EDGE ( 'NONE', *, *, #3481, .F. ) ;
#1143 = DIRECTION ( 'NONE',  ( 0.000000000000000000, 1.000000000000000000, 0.000000000000000000 ) ) ;
#1144 = CARTESIAN_POINT ( 'NONE',  ( 0.6676154558030191755, 0.02175203226844540927, -0.4667586584590060483 ) ) ;
#1145 = ORIENTED_EDGE ( 'NONE', *, *, #42, .T. ) ;
#1146 = CARTESIAN_POINT ( 'NONE',  ( 0.06299999999999994493, 1.679378605318059492, 1.679378605318041506 ) ) ;
#1147 = AXIS2_PLACEMENT_3D ( 'NONE', #11675, #1178, #24 ) ;
#1148 = CARTESIAN_POINT ( 'NONE',  ( 3.426491571325181340, 2.399999999999999911, -0.7000000000000007327 ) ) ;
#1149 = DIRECTION ( 'NONE',  ( 0.000000000000000000, 0.000000000000000000, -1.000000000000000000 ) ) ;
#1150 = CIRCLE ( 'NONE', #8730, 0.3750000000000004996 ) ;
#1151 = VERTEX_POINT ( 'NONE', #8422 ) ;
#1152 = CARTESIAN_POINT ( 'NONE',  ( 3.414222290118229974, 1.988642828590650780, -0.5921450265355728826 ) ) ;
#1153 = FACE_OUTER_BOUND ( 'NONE', #2958, .T. ) ;
#1154 = DIRECTION ( 'NONE',  ( 0.000000000000000000, 0.000000000000000000, 1.000000000000000000 ) ) ;
#1155 = ORIENTED_EDGE ( 'NONE', *, *, #12032, .T. ) ;
#1156 = DIRECTION ( 'NONE',  ( 1.000000000000000000, -0.000000000000000000, 1.224646799147353207E-16 ) ) ;
#1157 = EDGE_CURVE ( 'NONE', #8481, #7135, #6351, .T. ) ;
#1158 = ORIENTED_EDGE ( 'NONE', *, *, #5781, .F. ) ;
#1159 = CARTESIAN_POINT ( 'NONE',  ( 9.797174393178826150E-17, 0.000000000000000000, 0.8000000000000000444 ) ) ;
#1160 = VERTEX_POINT ( 'NONE', #2603 ) ;
#1161 = AXIS2_PLACEMENT_3D ( 'NONE', #7424, #6282, #434 ) ;
#1162 = DIRECTION ( 'NONE',  ( 0.9702019082525984439, 0.2422978687958614041, 1.188154661468198570E-16 ) ) ;
#1163 = CARTESIAN_POINT ( 'NONE',  ( 1.262572881824740367, -0.4300086559499006200, -0.4821670496918215032 ) ) ;
#1164 = DIRECTION ( 'NONE',  ( -0.7071067811865429098, 0.000000000000000000, 0.7071067811865521247 ) ) ;
#1165 = CIRCLE ( 'NONE', #6318, 1.000000000000000888 ) ;
#1166 = AXIS2_PLACEMENT_3D ( 'NONE', #3839, #10869, #14228 ) ;
#1167 = DIRECTION ( 'NONE',  ( -0.5000000000000041078, 0.000000000000000000, -0.8660254037844362651 ) ) ;
#1168 = EDGE_CURVE ( 'NONE', #10132, #1043, #205, .T. ) ;
#1169 = ADVANCED_FACE ( 'NONE', ( #4041 ), #1572, .F. ) ;
#1170 = ADVANCED_FACE ( 'NONE', ( #11573 ), #7964, .F. ) ;
#1171 = CIRCLE ( 'NONE', #2901, 2.500000000000000000 ) ;
#1172 = ORIENTED_EDGE ( 'NONE', *, *, #1481, .F. ) ;
#1173 = AXIS2_PLACEMENT_3D ( 'NONE', #6740, #11398, #668 ) ;
#1174 = EDGE_LOOP ( 'NONE', ( #232, #14316, #12026, #5429 ) ) ;
#1175 = AXIS2_PLACEMENT_3D ( 'NONE', #6897, #1132, #5822 ) ;
#1176 = PLANE ( 'NONE',  #13566 ) ;
#1177 = ORIENTED_EDGE ( 'NONE', *, *, #6713, .F. ) ;
#1178 = DIRECTION ( 'NONE',  ( 0.000000000000000000, 1.000000000000000000, 0.000000000000000000 ) ) ;
#1179 = CARTESIAN_POINT ( 'NONE',  ( 0.8722377123985701752, -0.4669784293568965405, -0.4449823291402679182 ) ) ;
#1181 = DIRECTION ( 'NONE',  ( 0.000000000000000000, 0.000000000000000000, -1.000000000000000000 ) ) ;
#1180 = AXIS2_PLACEMENT_3D ( 'NONE', #1875, #14665, #413 ) ;
#1182 = EDGE_CURVE ( 'NONE', #6882, #11005, #9441, .T. ) ;
#1183 = CARTESIAN_POINT ( 'NONE',  ( 3.394491571325183088, 1.679378605318059048, 1.941878605318041462 ) ) ;
#1184 = ORIENTED_EDGE ( 'NONE', *, *, #4862, .T. ) ;
#1185 = AXIS2_PLACEMENT_3D ( 'NONE', #12145, #10998, #490 ) ;
#1186 = DIRECTION ( 'NONE',  ( -0.000000000000000000, -1.000000000000000000, -0.000000000000000000 ) ) ;
#1187 = LINE ( 'NONE', #954, #6791 ) ;
#1188 = CARTESIAN_POINT ( 'NONE',  ( 3.875000000000000000, 1.112678268764263789, -0.4849999999999995981 ) ) ;
#1189 = AXIS2_PLACEMENT_3D ( 'NONE', #8652, #10947, #11020 ) ;
#1190 = AXIS2_PLACEMENT_3D ( 'NONE', #5397, #4093, #14338 ) ;
#1191 = CARTESIAN_POINT ( 'NONE',  ( -0.4125000000000001998, -0.6290000000000005587, -0.3725000000000000533 ) ) ;
#1192 = CARTESIAN_POINT ( 'NONE',  ( 4.587230667253597183, 1.743394675270711458, -0.2422858810294691856 ) ) ;
#1193 = VERTEX_POINT ( 'NONE', #10736 ) ;
#1195 = ORIENTED_EDGE ( 'NONE', *, *, #601, .T. ) ;
#1194 = DIRECTION ( 'NONE',  ( -1.000000000000000000, -0.000000000000000000, -0.000000000000000000 ) ) ;
#1196 = ORIENTED_EDGE ( 'NONE', *, *, #1286, .F. ) ;
#1197 = CARTESIAN_POINT ( 'NONE',  ( 5.546318247523970513, 0.000000000000000000, 1.502725933896874810 ) ) ;
#1198 = VERTEX_POINT ( 'NONE', #12020 ) ;
#1199 = CARTESIAN_POINT ( 'NONE',  ( 6.794491571325179891, 1.679378605318035733, -2.054378605318066153 ) ) ;
#1200 = CARTESIAN_POINT ( 'NONE',  ( 3.876618565749206713, 4.147999999999996135, 0.001734730694371304028 ) ) ;
#1201 = DIRECTION ( 'NONE',  ( 0.000000000000000000, 0.000000000000000000, -1.000000000000000000 ) ) ;
#1202 = ORIENTED_EDGE ( 'NONE', *, *, #8195, .T. ) ;
#1203 = AXIS2_PLACEMENT_3D ( 'NONE', #6983, #7973, #11644 ) ;
#1204 = CARTESIAN_POINT ( 'NONE',  ( -0.04538567959942197555, 1.602419810250338861, -0.3809527529760086684 ) ) ;
#1205 = CARTESIAN_POINT ( 'NONE',  ( -0.09035531712817639061, 1.379999999999999671, -0.1564999999999998892 ) ) ;
#1206 = EDGE_CURVE ( 'NONE', #10975, #1691, #225, .T. ) ;
#1207 = CIRCLE ( 'NONE', #9290, 0.4349999999999999978 ) ;
#1208 = CARTESIAN_POINT ( 'NONE',  ( 8.475037399843312613, 0.8689060174719044349, 0.3802960819231170908 ) ) ;
#1209 = CARTESIAN_POINT ( 'NONE',  ( 6.208491571325183145, -1.679378605318048390, 2.054378605318054607 ) ) ;
#1210 = EDGE_CURVE ( 'NONE', #2101, #6280, #8728, .T. ) ;
#1211 = DIRECTION ( 'NONE',  ( 0.000000000000000000, 0.000000000000000000, -1.000000000000000000 ) ) ;
#1212 = DIRECTION ( 'NONE',  ( 0.000000000000000000, 0.000000000000000000, 1.000000000000000000 ) ) ;
#1213 = CARTESIAN_POINT ( 'NONE',  ( 3.442233731549079412, 0.9679978390437318225, 0.2525149742857387691 ) ) ;
#1214 = CARTESIAN_POINT ( 'NONE',  ( 4.666407739276771771, 1.730062807210744902, 0.1714704599012415176 ) ) ;
#1215 = AXIS2_PLACEMENT_3D ( 'NONE', #2597, #6125, #8354 ) ;
#1216 = EDGE_LOOP ( 'NONE', ( #2848, #404, #9726, #8653 ) ) ;
#1217 = DIRECTION ( 'NONE',  ( -1.000000000000000000, -0.000000000000000000, -0.000000000000000000 ) ) ;
#1219 = ORIENTED_EDGE ( 'NONE', *, *, #5682, .F. ) ;
#1218 = DIRECTION ( 'NONE',  ( -1.000000000000000000, -0.000000000000000000, -0.000000000000000000 ) ) ;
#1220 = ORIENTED_EDGE ( 'NONE', *, *, #9053, .T. ) ;
#1221 = LINE ( 'NONE', #1292, #1649 ) ;
#1222 = DIRECTION ( 'NONE',  ( 0.000000000000000000, 0.000000000000000000, -1.000000000000000000 ) ) ;
#1223 = VERTEX_POINT ( 'NONE', #13084 ) ;
#1224 = DIRECTION ( 'NONE',  ( 1.365923996832131609E-16, -1.000000000000000000, -0.000000000000000000 ) ) ;
#1225 = ADVANCED_FACE ( 'NONE', ( #2621 ), #8300, .F. ) ;
#1226 = EDGE_CURVE ( 'NONE', #4411, #3185, #446, .T. ) ;
#1227 = DIRECTION ( 'NONE',  ( 1.000000000000000000, 0.000000000000000000, 0.000000000000000000 ) ) ;
#1228 = CARTESIAN_POINT ( 'NONE',  ( 0.06299999999999994493, 1.679378605318059492, 2.086378605318047086 ) ) ;
#1229 = VERTEX_POINT ( 'NONE', #293 ) ;
#1230 = CARTESIAN_POINT ( 'NONE',  ( 0.6601485485260575325, -0.3723516483516470243, 0.5137583810202325241 ) ) ;
#1231 = FACE_OUTER_BOUND ( 'NONE', #14908, .T. ) ;
#1232 = CARTESIAN_POINT ( 'NONE',  ( 2.124999999999999556, -1.679378605318059048, -1.679378605318041950 ) ) ;
#1233 = EDGE_LOOP ( 'NONE', ( #7766, #3078, #5605, #10462 ) ) ;
#1234 = CIRCLE ( 'NONE', #9570, 0.1899999999999996136 ) ;
#1235 = CARTESIAN_POINT ( 'NONE',  ( 3.405153689607044232, 2.750000000000000000, 1.491010071662831171 ) ) ;
#1236 = ORIENTED_EDGE ( 'NONE', *, *, #12925, .T. ) ;
#1237 = DIRECTION ( 'NONE',  ( -1.000000000000000000, -0.000000000000000000, -0.000000000000000000 ) ) ;
#1238 = ORIENTED_EDGE ( 'NONE', *, *, #12127, .F. ) ;
#1239 = LINE ( 'NONE', #5927, #8683 ) ;
#1240 = CARTESIAN_POINT ( 'NONE',  ( 1.000847373107695226, -0.4430000000000000049, -0.4858637376679705855 ) ) ;
#1241 = CARTESIAN_POINT ( 'NONE',  ( 0.09035531712817648775, 1.379999999999999671, -0.1564999999999998892 ) ) ;
#1242 = CIRCLE ( 'NONE', #4437, 0.07999999999999996003 ) ;
#1243 = EDGE_CURVE ( 'NONE', #8971, #5394, #3645, .T. ) ;
#1244 = DIRECTION ( 'NONE',  ( 0.000000000000000000, -0.7071067811865509034, -0.7071067811865441310 ) ) ;
#1245 = CARTESIAN_POINT ( 'NONE',  ( 3.708475701238409528, 1.919230964417490748, -0.7311178887250847636 ) ) ;
#1246 = EDGE_LOOP ( 'NONE', ( #2787, #5368, #4334, #7319 ) ) ;
#1247 = ORIENTED_EDGE ( 'NONE', *, *, #8778, .T. ) ;
#1248 = UNCERTAINTY_MEASURE_WITH_UNIT (LENGTH_MEASURE( 1.000000000000000082E-05 ), #2906, 'distance_accuracy_value', 'NONE');
#1249 = DIRECTION ( 'NONE',  ( 1.000000000000000000, -0.000000000000000000, -0.000000000000000000 ) ) ;
#1250 = CIRCLE ( 'NONE', #8375, 1.350000000000000089 ) ;
#1251 = DIRECTION ( 'NONE',  ( 0.000000000000000000, -1.000000000000000000, 0.000000000000000000 ) ) ;
#1252 = CARTESIAN_POINT ( 'NONE',  ( 0.8502743344449713581, -0.4776025933964622716, -0.4315470089081906435 ) ) ;
#1253 = FACE_OUTER_BOUND ( 'NONE', #6147, .T. ) ;
#1254 = CARTESIAN_POINT ( 'NONE',  ( 0.7058998964907862161, -0.05999999999999994227, -0.4900296624789436950 ) ) ;
#1255 = ORIENTED_EDGE ( 'NONE', *, *, #7916, .T. ) ;
#1256 = CARTESIAN_POINT ( 'NONE',  ( 3.632032016703825583, 1.941006471662596322, -0.4371510339114678123 ) ) ;
#1257 = EDGE_CURVE ( 'NONE', #8991, #4134, #5598, .T. ) ;
#1258 = PLANE ( 'NONE',  #10237 ) ;
#1259 = CARTESIAN_POINT ( 'NONE',  ( 3.874999999999999556, 3.535499999999999421, -1.320000000000000062 ) ) ;
#1260 = DIRECTION ( 'NONE',  ( 0.000000000000000000, 0.000000000000000000, 1.000000000000000000 ) ) ;
#1261 = DIRECTION ( 'NONE',  ( -0.000000000000000000, -1.000000000000000000, -0.000000000000000000 ) ) ;
#1262 = EDGE_CURVE ( 'NONE', #2201, #14331, #2840, .T. ) ;
#1263 = CARTESIAN_POINT ( 'NONE',  ( 4.685225399282611392, 1.733178264597110552, -0.03635724695066767931 ) ) ;
#1264 = ORIENTED_EDGE ( 'NONE', *, *, #5714, .F. ) ;
#1266 = ORIENTED_EDGE ( 'NONE', *, *, #8453, .F. ) ;
#1265 = CARTESIAN_POINT ( 'NONE',  ( 3.944129661530210385, 0.000000000000000000, 1.932031071636253650 ) ) ;
#1267 = ORIENTED_EDGE ( 'NONE', *, *, #940, .T. ) ;
#1268 = LINE ( 'NONE', #8266, #13818 ) ;
#1269 = ORIENTED_EDGE ( 'NONE', *, *, #2217, .F. ) ;
#1270 = CIRCLE ( 'NONE', #8136, 0.2945000000000009277 ) ;
#1271 = CYLINDRICAL_SURFACE ( 'NONE', #15075, 3.000000000000000444 ) ;
#1272 = DIRECTION ( 'NONE',  ( -4.619079197907164195E-18, 0.8397743105139239272, -0.5429356383595238533 ) ) ;
#1273 = CYLINDRICAL_SURFACE ( 'NONE', #11108, 0.2812500000000000555 ) ;
#1274 = VERTEX_POINT ( 'NONE', #6369 ) ;
#1275 = CARTESIAN_POINT ( 'NONE',  ( 8.474190026735612946, 1.056999999999999940, 0.3203020658980470503 ) ) ;
#1276 = LINE ( 'NONE', #4820, #14380 ) ;
#1277 = EDGE_CURVE ( 'NONE', #1362, #5506, #13882, .T. ) ;
#1278 = CARTESIAN_POINT ( 'NONE',  ( 0.09500000000000431710, 1.679378605318035733, -1.304378605318064821 ) ) ;
#1279 = EDGE_CURVE ( 'NONE', #14026, #1062, #10731, .T. ) ;
#1280 = DIRECTION ( 'NONE',  ( 0.000000000000000000, 0.000000000000000000, -1.000000000000000000 ) ) ;
#1281 = PLANE ( 'NONE',  #10902 ) ;
#1282 = DIRECTION ( 'NONE',  ( 1.000000000000000000, 0.000000000000000000, 0.000000000000000000 ) ) ;
#1283 = EDGE_CURVE ( 'NONE', #6530, #498, #12667, .T. ) ;
#1284 = CARTESIAN_POINT ( 'NONE',  ( 2.124999999999999556, -1.679378605318041950, 1.679378605318059048 ) ) ;
#1285 = CARTESIAN_POINT ( 'NONE',  ( 4.685864643020170917, 1.733287931739606380, 0.04932201671138494725 ) ) ;
#1286 = EDGE_CURVE ( 'NONE', #1997, #2748, #14528, .T. ) ;
#1287 = ORIENTED_EDGE ( 'NONE', *, *, #12402, .F. ) ;
#1288 = DIRECTION ( 'NONE',  ( 0.7071067811865612285, 0.7071067811865339170, -1.170732267570244050E-16 ) ) ;
#1290 = ORIENTED_EDGE ( 'NONE', *, *, #6124, .T. ) ;
#1289 = FACE_OUTER_BOUND ( 'NONE', #8073, .T. ) ;
#1291 = EDGE_LOOP ( 'NONE', ( #2563, #9836, #6390, #2394 ) ) ;
#1292 = CARTESIAN_POINT ( 'NONE',  ( 2.980731298636167370, 3.567999999999999616, 0.3249191361593796179 ) ) ;
#1293 = CARTESIAN_POINT ( 'NONE',  ( 3.897879830116474320, 1.879038604582284666, 0.5000000000000002220 ) ) ;
#1294 = CYLINDRICAL_SURFACE ( 'NONE', #6715, 0.1250000000000000278 ) ;
#1295 = ORIENTED_EDGE ( 'NONE', *, *, #8058, .F. ) ;
#1296 = DIRECTION ( 'NONE',  ( 0.000000000000000000, 1.000000000000000000, 0.000000000000000000 ) ) ;
#1297 = CYLINDRICAL_SURFACE ( 'NONE', #12565, 0.3750000000000004996 ) ;
#1298 = AXIS2_PLACEMENT_3D ( 'NONE', #9493, #12988, #14142 ) ;
#1299 = FACE_OUTER_BOUND ( 'NONE', #7207, .T. ) ;
#1300 = EDGE_CURVE ( 'NONE', #2080, #5889, #11936, .T. ) ;
#1301 = AXIS2_PLACEMENT_3D ( 'NONE', #15094, #14094, #3628 ) ;
#1302 = ORIENTED_EDGE ( 'NONE', *, *, #9073, .T. ) ;
#1303 = DIRECTION ( 'NONE',  ( 1.655665450705613915E-16, 0.000000000000000000, 1.000000000000000000 ) ) ;
#1304 = CARTESIAN_POINT ( 'NONE',  ( 0.6733128806866760518, -0.4720829350095157029, 0.4545362700951272594 ) ) ;
#1305 = DIRECTION ( 'NONE',  ( 0.000000000000000000, 0.000000000000000000, 1.000000000000000000 ) ) ;
#1306 = DIRECTION ( 'NONE',  ( 0.000000000000000000, 0.000000000000000000, -1.000000000000000000 ) ) ;
#1307 = EDGE_LOOP ( 'NONE', ( #12654, #10142, #11894, #4155 ) ) ;
#1308 = CARTESIAN_POINT ( 'NONE',  ( 2.650000000000001688, 0.000000000000000000, 1.000000000000000000 ) ) ;
#1309 = CARTESIAN_POINT ( 'NONE',  ( 0.3724999999999997757, 0.1859999999999983611, -0.4125000000000000333 ) ) ;
#1310 = ORIENTED_EDGE ( 'NONE', *, *, #14979, .F. ) ;
#1311 = EDGE_CURVE ( 'NONE', #11971, #13813, #11437, .T. ) ;
#1312 = DIRECTION ( 'NONE',  ( -0.000000000000000000, 4.591341165821852610E-16, -1.000000000000000000 ) ) ;
#1313 = VERTEX_POINT ( 'NONE', #517 ) ;
#1314 = AXIS2_PLACEMENT_3D ( 'NONE', #2218, #10263, #903 ) ;
#1315 = DIRECTION ( 'NONE',  ( 0.000000000000000000, -1.000000000000000000, 0.000000000000000000 ) ) ;
#1316 = CARTESIAN_POINT ( 'NONE',  ( 1.973079680967599892, -0.1265933021011455828, -0.4721316429241865231 ) ) ;
#1317 = CARTESIAN_POINT ( 'NONE',  ( 1.000847373107697891, -0.3830000000000000071, 0.4858637376679703634 ) ) ;
#1318 = FACE_OUTER_BOUND ( 'NONE', #8544, .T. ) ;
#1319 = CIRCLE ( 'NONE', #9883, 1.812500000000000222 ) ;
#1320 = DIRECTION ( 'NONE',  ( -1.000000000000000000, -0.000000000000000000, -0.000000000000000000 ) ) ;
#1321 = ORIENTED_EDGE ( 'NONE', *, *, #7727, .F. ) ;
#1322 = EDGE_LOOP ( 'NONE', ( #5245, #3256, #6400, #5138 ) ) ;
#1323 = ORIENTED_EDGE ( 'NONE', *, *, #5681, .T. ) ;
#1324 = EDGE_CURVE ( 'NONE', #1733, #10897, #5794, .T. ) ;
#1325 = LINE ( 'NONE', #1403, #3569 ) ;
#1326 = DIRECTION ( 'NONE',  ( 3.824587191129971267E-15, 0.000000000000000000, -1.000000000000000000 ) ) ;
#1327 = CARTESIAN_POINT ( 'NONE',  ( 3.444319122601930972E-17, 1.591999999999999638, 0.2812500000000000555 ) ) ;
#1328 = TOROIDAL_SURFACE ( 'NONE', #9665, 1.552690549202460968, 0.05999999999999999778 ) ;
#1329 = CARTESIAN_POINT ( 'NONE',  ( 0.8999999999999999112, -0.6429999999999999050, -0.4300000000000014921 ) ) ;
#1330 = ORIENTED_EDGE ( 'NONE', *, *, #11282, .T. ) ;
#1331 = CARTESIAN_POINT ( 'NONE',  ( 0.1250000000000009992, 0.000000000000000000, 0.000000000000000000 ) ) ;
#1332 = AXIS2_PLACEMENT_3D ( 'NONE', #13543, #4164, #13625 ) ;
#1333 = CARTESIAN_POINT ( 'NONE',  ( 2.045495128834869725, 0.3295048711651374362, 0.4105035982572215469 ) ) ;
#1334 = FACE_OUTER_BOUND ( 'NONE', #477, .T. ) ;
#1335 = CARTESIAN_POINT ( 'NONE',  ( 0.3724999999999999423, -0.6589999999999996971, 0.4424999999999982836 ) ) ;
#1336 = CIRCLE ( 'NONE', #13781, 0.1050000000000006622 ) ;
#1337 = ORIENTED_EDGE ( 'NONE', *, *, #7310, .F. ) ;
#1338 = AXIS2_PLACEMENT_3D ( 'NONE', #13018, #2555, #11162 ) ;
#1340 = ORIENTED_EDGE ( 'NONE', *, *, #12955, .T. ) ;
#1339 = CARTESIAN_POINT ( 'NONE',  ( 0.2249147617188453907, 1.559103846021540951, 0.3723417112827335784 ) ) ;
#1341 = CIRCLE ( 'NONE', #7465, 0.2625000000000000111 ) ;
#1342 = VERTEX_POINT ( 'NONE', #3923 ) ;
#1343 = CARTESIAN_POINT ( 'NONE',  ( 2.774999999999999911, -1.575000000000000178, 2.360000000000016751 ) ) ;
#1344 = ORIENTED_EDGE ( 'NONE', *, *, #10558, .F. ) ;
#1345 = FACE_OUTER_BOUND ( 'NONE', #3353, .T. ) ;
#1346 = APPLICATION_PROTOCOL_DEFINITION ( 'draft international standard', 'automotive_design', 1998, #12307 ) ;
#1347 = DIRECTION ( 'NONE',  ( 1.000000000000000000, 0.000000000000000000, 0.000000000000000000 ) ) ;
#1348 = VERTEX_POINT ( 'NONE', #3846 ) ;
#1349 = DIRECTION ( 'NONE',  ( 0.000000000000000000, 0.000000000000000000, 1.000000000000000000 ) ) ;
#1350 = DIRECTION ( 'NONE',  ( 0.000000000000000000, -1.000000000000000000, 0.000000000000000000 ) ) ;
#1351 = AXIS2_PLACEMENT_3D ( 'NONE', #14861, #11653, #7986 ) ;
#1352 = CARTESIAN_POINT ( 'NONE',  ( 3.793823152521890840, 1.884745230718079423, 0.7457052748579492407 ) ) ;
#1353 = AXIS2_PLACEMENT_3D ( 'NONE', #644, #564, #11000 ) ;
#1354 = CIRCLE ( 'NONE', #11881, 0.5000000000000000000 ) ;
#1355 = CYLINDRICAL_SURFACE ( 'NONE', #14795, 0.1899999999999996136 ) ;
#1356 = PLANE ( 'NONE',  #4864 ) ;
#1357 = DIRECTION ( 'NONE',  ( -1.000000000000000000, -0.000000000000000000, -0.000000000000000000 ) ) ;
#1358 = EDGE_CURVE ( 'NONE', #12028, #12407, #2764, .T. ) ;
#1359 = CARTESIAN_POINT ( 'NONE',  ( 4.609856173843976279, 1.721777932115673426, 0.3359333493936877413 ) ) ;
#1360 = EDGE_CURVE ( 'NONE', #9406, #3272, #9661, .T. ) ;
#1361 = AXIS2_PLACEMENT_3D ( 'NONE', #4299, #12538, #3222 ) ;
#1362 = VERTEX_POINT ( 'NONE', #14311 ) ;
#1363 = EDGE_CURVE ( 'NONE', #799, #11919, #10951, .T. ) ;
#1364 = DIRECTION ( 'NONE',  ( -0.000000000000000000, -1.000000000000000000, -0.000000000000000000 ) ) ;
#1366 = ORIENTED_EDGE ( 'NONE', *, *, #12214, .F. ) ;
#1365 = DIRECTION ( 'NONE',  ( 0.000000000000000000, 1.000000000000000000, 0.000000000000000000 ) ) ;
#1367 = ORIENTED_EDGE ( 'NONE', *, *, #4089, .T. ) ;
#1368 = DIRECTION ( 'NONE',  ( 0.000000000000000000, 0.000000000000000000, -1.000000000000000000 ) ) ;
#1369 = DIRECTION ( 'NONE',  ( 0.000000000000000000, 0.000000000000000000, 1.000000000000000000 ) ) ;
#1370 = ORIENTED_EDGE ( 'NONE', *, *, #14359, .F. ) ;
#1371 = DIRECTION ( 'NONE',  ( -1.000000000000000000, -0.000000000000000000, -0.000000000000000000 ) ) ;
#1372 = EDGE_CURVE ( 'NONE', #9682, #12434, #9016, .T. ) ;
#1373 = EDGE_CURVE ( 'NONE', #9926, #14596, #8810, .T. ) ;
#1374 = VECTOR ( 'NONE', #1731, 39.37007874015748143 ) ;
#1375 = DIRECTION ( 'NONE',  ( -0.9999002670844991947, 0.000000000000000000, -0.01412288512831128343 ) ) ;
#1376 = CARTESIAN_POINT ( 'NONE',  ( 0.4424999999999982281, -0.6589999999999996971, 0.3724999999999999423 ) ) ;
#1377 = ORIENTED_EDGE ( 'NONE', *, *, #8091, .F. ) ;
#1378 = PLANE ( 'NONE',  #2724 ) ;
#1379 = CARTESIAN_POINT ( 'NONE',  ( 3.341312140645306794, 1.997119961756267603, -0.6280817267650429248 ) ) ;
#1380 = AXIS2_PLACEMENT_3D ( 'NONE', #8031, #11306, #6581 ) ;
#1381 = CARTESIAN_POINT ( 'NONE',  ( 8.849152626892301754, -0.05999999999999997696, 0.3150059839749300705 ) ) ;
#1382 = LINE ( 'NONE', #11804, #13153 ) ;
#1383 = ORIENTED_EDGE ( 'NONE', *, *, #3442, .T. ) ;
#1384 = PRODUCT_DEFINITION_SHAPE ( 'NONE', 'NONE',  #15158 ) ;
#1385 = DIRECTION ( 'NONE',  ( -1.000000000000000000, -0.000000000000000000, -0.000000000000000000 ) ) ;
#1386 = VERTEX_POINT ( 'NONE', #5515 ) ;
#1387 = CIRCLE ( 'NONE', #14093, 1.500000000000000222 ) ;
#1388 = CARTESIAN_POINT ( 'NONE',  ( 6.794491571325179891, -1.679378605318047946, -1.679378605318053497 ) ) ;
#1389 = ORIENTED_EDGE ( 'NONE', *, *, #8998, .T. ) ;
#1390 = DIRECTION ( 'NONE',  ( -1.000000000000000000, -0.000000000000000000, -0.000000000000000000 ) ) ;
#1391 = CARTESIAN_POINT ( 'NONE',  ( 0.9652705920801474271, -0.4828330467331338749, -0.4119425203458967344 ) ) ;
#1392 = VECTOR ( 'NONE', #8781, 39.37007874015748143 ) ;
#1393 = EDGE_CURVE ( 'NONE', #8887, #9027, #9003, .T. ) ;
#1394 = DIRECTION ( 'NONE',  ( 1.000000000000000000, 0.000000000000000000, 0.000000000000000000 ) ) ;
#1395 = DIRECTION ( 'NONE',  ( 1.000000000000000000, 0.000000000000000000, 0.000000000000000000 ) ) ;
#1396 = EDGE_CURVE ( 'NONE', #8780, #1562, #5587, .T. ) ;
#1397 = LINE ( 'NONE', #4940, #6984 ) ;
#1398 = CIRCLE ( 'NONE', #15093, 0.3750000000000004996 ) ;
#1399 = ORIENTED_EDGE ( 'NONE', *, *, #6616, .F. ) ;
#1400 = ORIENTED_EDGE ( 'NONE', *, *, #12508, .T. ) ;
#1401 = AXIS2_PLACEMENT_3D ( 'NONE', #4356, #7718, #9097 ) ;
#1402 = ORIENTED_EDGE ( 'NONE', *, *, #5015, .F. ) ;
#1403 = CARTESIAN_POINT ( 'NONE',  ( 0.000000000000000000, 0.000000000000000000, -0.1900000000000000577 ) ) ;
#1404 = CARTESIAN_POINT ( 'NONE',  ( 0.7100000000000001865, 0.000000000000000000, 1.552690549202460968 ) ) ;
#1405 = DIRECTION ( 'NONE',  ( 0.000000000000000000, 0.000000000000000000, -1.000000000000000000 ) ) ;
#1406 = CARTESIAN_POINT ( 'NONE',  ( 0.7096982392392988670, -0.01548513119911374726, -0.4703908291968748046 ) ) ;
#1407 = ORIENTED_EDGE ( 'NONE', *, *, #8888, .F. ) ;
#1408 = VECTOR ( 'NONE', #8253, 39.37007874015748143 ) ;
#1409 = DIRECTION ( 'NONE',  ( -0.000000000000000000, 1.000000000000000000, -0.000000000000000000 ) ) ;
#1410 = CIRCLE ( 'NONE', #4364, 0.03999999999999998002 ) ;
#1411 = CARTESIAN_POINT ( 'NONE',  ( 1.324514161726516592, 5.548674797643638688E-05, 0.4812921728570948576 ) ) ;
#1412 = EDGE_CURVE ( 'NONE', #1001, #6235, #9956, .T. ) ;
#1413 = EDGE_CURVE ( 'NONE', #9216, #3261, #12518, .T. ) ;
#1414 = FACE_OUTER_BOUND ( 'NONE', #7633, .T. ) ;
#1415 = AXIS2_PLACEMENT_3D ( 'NONE', #5157, #240, #4939 ) ;
#1416 = CIRCLE ( 'NONE', #3151, 0.06000000000000002554 ) ;
#1417 = AXIS2_PLACEMENT_3D ( 'NONE', #2473, #14168, #3540 ) ;
#1418 = ORIENTED_EDGE ( 'NONE', *, *, #8906, .F. ) ;
#1420 = ORIENTED_EDGE ( 'NONE', *, *, #12128, .T. ) ;
#1419 = DIRECTION ( 'NONE',  ( 0.000000000000000000, 1.000000000000000000, 0.000000000000000000 ) ) ;
#1421 = AXIS2_PLACEMENT_3D ( 'NONE', #7428, #5983, #10944 ) ;
#1422 = VERTEX_POINT ( 'NONE', #14761 ) ;
#1423 = CARTESIAN_POINT ( 'NONE',  ( 0.1702285915635917413, 1.581112972951822293, 0.3809527529760086684 ) ) ;
#1424 = ORIENTED_EDGE ( 'NONE', *, *, #2865, .F. ) ;
#1425 = CARTESIAN_POINT ( 'NONE',  ( 2.775039370078740131, 1.679378605318059492, 1.679378605318041506 ) ) ;
#1426 = APPLICATION_PROTOCOL_DEFINITION ( 'draft international standard', 'automotive_design', 1998, #13279 ) ;
#1427 = CARTESIAN_POINT ( 'NONE',  ( 2.774999999999999911, 2.359999999999993214, -1.575000000000016831 ) ) ;
#1428 = ORIENTED_EDGE ( 'NONE', *, *, #10238, .F. ) ;
#1429 = AXIS2_PLACEMENT_3D ( 'NONE', #10033, #7649, #14691 ) ;
#1430 = CARTESIAN_POINT ( 'NONE',  ( 8.469665986256828205, 0.9969999999999998863, 6.829619984160658046E-17 ) ) ;
#1431 = LINE ( 'NONE', #7410, #5606 ) ;
#1432 = CIRCLE ( 'NONE', #4374, 0.05500000000000146438 ) ;
#1433 = DIRECTION ( 'NONE',  ( 0.000000000000000000, 1.000000000000000000, 0.000000000000000000 ) ) ;
#1434 = AXIS2_PLACEMENT_3D ( 'NONE', #2990, #7655, #3849 ) ;
#1435 = VECTOR ( 'NONE', #12984, 39.37007874015748143 ) ;
#1436 = CIRCLE ( 'NONE', #10003, 0.08500000000000004774 ) ;
#1437 = EDGE_CURVE ( 'NONE', #11419, #1348, #7787, .T. ) ;
#1438 = FACE_BOUND ( 'NONE', #2610, .T. ) ;
#1439 = CARTESIAN_POINT ( 'NONE',  ( 0.8091754559563963944, -0.4422237819269027037, -0.4392762457493078476 ) ) ;
#1440 = CARTESIAN_POINT ( 'NONE',  ( 3.563446790140585740, 1.891298529660668137, 0.7485675892123550002 ) ) ;
#1441 = DIRECTION ( 'NONE',  ( 0.000000000000000000, 1.000000000000000000, 0.000000000000000000 ) ) ;
#1442 = ORIENTED_EDGE ( 'NONE', *, *, #13709, .F. ) ;
#1443 = CARTESIAN_POINT ( 'NONE',  ( 0.6676154558030189534, -0.4647520322684451366, 0.4667586584590060483 ) ) ;
#1445 = EDGE_LOOP ( 'NONE', ( #6924, #6300, #212, #4258 ) ) ;
#1444 = LINE ( 'NONE', #10494, #3327 ) ;
#1446 = ORIENTED_EDGE ( 'NONE', *, *, #3949, .T. ) ;
#1447 = AXIS2_PLACEMENT_3D ( 'NONE', #8996, #11278, #14794 ) ;
#1448 = DIRECTION ( 'NONE',  ( -0.000000000000000000, -1.000000000000000000, -0.000000000000000000 ) ) ;
#1449 =( CONVERSION_BASED_UNIT ( 'INCH', #215 ) LENGTH_UNIT ( ) NAMED_UNIT ( #10871 ) );
#1450 = CARTESIAN_POINT ( 'NONE',  ( 2.916325821605814106, 0.5706613545855653280, 0.3991895006237018428 ) ) ;
#1451 = EDGE_LOOP ( 'NONE', ( #10714, #8361, #4810, #7280 ) ) ;
#1452 = LINE ( 'NONE', #5140, #13383 ) ;
#1453 = EDGE_CURVE ( 'NONE', #6687, #1997, #4112, .T. ) ;
#1454 = FACE_BOUND ( 'NONE', #14206, .T. ) ;
#1455 = EDGE_CURVE ( 'NONE', #10371, #10000, #4614, .T. ) ;
#1456 = DIRECTION ( 'NONE',  ( 1.000000000000000000, 1.874307916738609066E-16, 0.000000000000000000 ) ) ;
#1457 = VECTOR ( 'NONE', #6225, 39.37007874015748143 ) ;
#1458 = ORIENTED_EDGE ( 'NONE', *, *, #8228, .F. ) ;
#1459 = DIRECTION ( 'NONE',  ( -1.000000000000000000, -0.000000000000000000, -0.000000000000000000 ) ) ;
#1460 = FACE_OUTER_BOUND ( 'NONE', #5577, .T. ) ;
#1461 = CARTESIAN_POINT ( 'NONE',  ( 2.774999999999999911, 3.360000000000000320, -0.9800000000000012035 ) ) ;
#1462 = ORIENTED_EDGE ( 'NONE', *, *, #7095, .F. ) ;
#1463 = DIRECTION ( 'NONE',  ( -0.000000000000000000, -1.000000000000000000, -0.000000000000000000 ) ) ;
#1464 = ADVANCED_FACE ( 'NONE', ( #14693 ), #13750, .T. ) ;
#1465 = AXIS2_PLACEMENT_3D ( 'NONE', #14897, #11605, #4725 ) ;
#1466 = CARTESIAN_POINT ( 'NONE',  ( 3.874999999999999556, 3.535499999999999421, 1.509999999999999787 ) ) ;
#1467 = EDGE_LOOP ( 'NONE', ( #12906, #13377, #12539, #4430 ) ) ;
#1468 = CARTESIAN_POINT ( 'NONE',  ( 0.3724999999999997757, -0.6589999999999996971, -0.4424999999999983391 ) ) ;
#1469 = ORIENTED_EDGE ( 'NONE', *, *, #14409, .T. ) ;
#1470 = DIRECTION ( 'NONE',  ( -1.000000000000000000, -0.000000000000000000, -0.000000000000000000 ) ) ;
#1471 = ADVANCED_FACE ( 'NONE', ( #13603 ), #12532, .T. ) ;
#1472 = PLANE ( 'NONE',  #7765 ) ;
#1473 = EDGE_CURVE ( 'NONE', #10245, #5661, #11168, .T. ) ;
#1474 = CARTESIAN_POINT ( 'NONE',  ( 3.944129661530210385, 1.761538328845252188, 0.7935532608319412207 ) ) ;
#1475 = LINE ( 'NONE', #6229, #346 ) ;
#1476 = COLOUR_RGB ( '',0.7921568627450980005, 0.8196078431372548767, 0.9333333333333333481 ) ;
#1477 = LINE ( 'NONE', #7751, #13206 ) ;
#1478 = ORIENTED_EDGE ( 'NONE', *, *, #6197, .F. ) ;
#1479 = EDGE_LOOP ( 'NONE', ( #11498, #12621 ) ) ;
#1480 = EDGE_LOOP ( 'NONE', ( #14975, #7023, #500, #8833 ) ) ;
#1481 = EDGE_CURVE ( 'NONE', #12926, #7285, #11319, .T. ) ;
#1482 = CARTESIAN_POINT ( 'NONE',  ( 8.752374375191426026, 0.8785908380595726097, -0.1599881670920904608 ) ) ;
#1483 = CARTESIAN_POINT ( 'NONE',  ( 0.09500000000000168032, 0.000000000000000000, 3.000000000000000444 ) ) ;
#1484 = DIRECTION ( 'NONE',  ( 0.000000000000000000, 0.000000000000000000, 1.000000000000000000 ) ) ;
#1485 = ADVANCED_FACE ( 'NONE', ( #10037 ), #2051, .F. ) ;
#1486 = CARTESIAN_POINT ( 'NONE',  ( 0.8999999999999998002, 0.1549999999999996103, -0.3799999999999999489 ) ) ;
#1487 = FACE_OUTER_BOUND ( 'NONE', #6810, .T. ) ;
#1488 = DIRECTION ( 'NONE',  ( 0.000000000000000000, 0.000000000000000000, -1.000000000000000000 ) ) ;
#1489 =( CONVERSION_BASED_UNIT ( 'INCH', #7745 ) LENGTH_UNIT ( ) NAMED_UNIT ( #3840 ) );
#1490 = ADVANCED_FACE ( 'NONE', ( #3217 ), #9109, .T. ) ;
#1491 = VECTOR ( 'NONE', #9688, 39.37007874015748143 ) ;
#1492 = CARTESIAN_POINT ( 'NONE',  ( 4.427625859550793130, 1.707399566347088449, -0.5781646599430360078 ) ) ;
#1493 = EDGE_LOOP ( 'NONE', ( #8132, #10838, #10009, #10420 ) ) ;
#1495 = ORIENTED_EDGE ( 'NONE', *, *, #2305, .T. ) ;
#1494 = CARTESIAN_POINT ( 'NONE',  ( 2.742999999999998995, -1.679378605318059048, -1.679378605318041950 ) ) ;
#1496 = ORIENTED_EDGE ( 'NONE', *, *, #9756, .F. ) ;
#1497 = DIRECTION ( 'NONE',  ( 1.000000000000000000, 0.000000000000000000, 0.000000000000000000 ) ) ;
#1498 = DIRECTION ( 'NONE',  ( -0.000000000000000000, -1.000000000000000000, -0.000000000000000000 ) ) ;
#1499 = EDGE_CURVE ( 'NONE', #10819, #14903, #4361, .T. ) ;
#1500 = APPLICATION_PROTOCOL_DEFINITION ( 'draft international standard', 'automotive_design', 1998, #6078 ) ;
#1501 = FACE_OUTER_BOUND ( 'NONE', #9427, .T. ) ;
#1502 = ORIENTED_EDGE ( 'NONE', *, *, #4020, .F. ) ;
#1503 = CARTESIAN_POINT ( 'NONE',  ( -0.1264631971972069724, 1.593677921218987992, -0.3809527529760086684 ) ) ;
#1504 = CARTESIAN_POINT ( 'NONE',  ( 3.944129661530210385, 0.000000000000000000, 1.932031071636253650 ) ) ;
#1505 = CARTESIAN_POINT ( 'NONE',  ( 3.876560711617219379, 2.749999999999999556, 0.7500000000000001110 ) ) ;
#1506 = CONICAL_SURFACE ( 'NONE', #3475, 0.2624999999999997335, 0.7853981633974419507 ) ;
#1507 = DIRECTION ( 'NONE',  ( 0.000000000000000000, 0.000000000000000000, -1.000000000000000000 ) ) ;
#1508 = FACE_BOUND ( 'NONE', #8831, .T. ) ;
#1509 = DIRECTION ( 'NONE',  ( 0.000000000000000000, 0.000000000000000000, 1.000000000000000000 ) ) ;
#1510 = CARTESIAN_POINT ( 'NONE',  ( 3.612336255711126931, 1.963150234975052033, 0.7021133243488046904 ) ) ;
#1511 = CARTESIAN_POINT ( 'NONE',  ( 3.426491571325181340, 2.399999999999999911, -0.7000000000000007327 ) ) ;
#1512 = AXIS2_PLACEMENT_3D ( 'NONE', #901, #5372, #8962 ) ;
#1513 =( BOUNDED_CURVE ( )  B_SPLINE_CURVE ( 3, ( #1690, #378, #12100, #5078 ),
 .UNSPECIFIED., .F., .F. ) 
 B_SPLINE_CURVE_WITH_KNOTS ( ( 4, 4 ),
 ( 4.712388980384689674, 5.497787143782138841 ),
 .UNSPECIFIED. ) 
 CURVE ( )  GEOMETRIC_REPRESENTATION_ITEM ( )  RATIONAL_B_SPLINE_CURVE ( ( 1.000000000000000000, 0.9492530216741910110, 0.9492530216741910110, 1.000000000000000000 ) ) 
 REPRESENTATION_ITEM ( '' )  );
#1514 = ORIENTED_EDGE ( 'NONE', *, *, #13348, .F. ) ;
#1515 = FACE_OUTER_BOUND ( 'NONE', #15108, .T. ) ;
#1517 = ORIENTED_EDGE ( 'NONE', *, *, #15120, .F. ) ;
#1516 = CYLINDRICAL_SURFACE ( 'NONE', #6025, 0.3750000000000007772 ) ;
#1518 = ORIENTED_EDGE ( 'NONE', *, *, #2556, .F. ) ;
#1519 = DIRECTION ( 'NONE',  ( -1.000000000000000000, -0.000000000000000000, -0.000000000000000000 ) ) ;
#1520 = EDGE_CURVE ( 'NONE', #5710, #10938, #914, .T. ) ;
#1521 = DIRECTION ( 'NONE',  ( 1.000000000000000000, 0.000000000000000000, 0.000000000000000000 ) ) ;
#1522 = CARTESIAN_POINT ( 'NONE',  ( 3.025735579118525198, 0.6832920890236183764, 0.4572636217638626488 ) ) ;
#1523 = EDGE_LOOP ( 'NONE', ( #7284, #1075, #6871, #10896 ) ) ;
#1524 = AXIS2_PLACEMENT_3D ( 'NONE', #8099, #2266, #10536 ) ;
#1525 = PRODUCT_DEFINITION ( 'UNKNOWN', '', #11843, #3110 ) ;
#1526 = CARTESIAN_POINT ( 'NONE',  ( 0.9659737678069143518, -0.4829423716508983166, -0.4107001390575403810 ) ) ;
#1527 = VECTOR ( 'NONE', #13580, 39.37007874015748143 ) ;
#1528 = CARTESIAN_POINT ( 'NONE',  ( 0.5400755080658357077, 0.000000000000000000, -1.657626322880899616 ) ) ;
#1529 = CARTESIAN_POINT ( 'NONE',  ( 0.000000000000000000, 0.1749999999999999889, 0.000000000000000000 ) ) ;
#1530 = ORIENTED_EDGE ( 'NONE', *, *, #12684, .T. ) ;
#1531 = CARTESIAN_POINT ( 'NONE',  ( 3.394491571325180423, -1.679378605318059048, -1.679378605318041950 ) ) ;
#1532 = DIRECTION ( 'NONE',  ( -1.655665450705613915E-16, -3.103226861728128995E-32, -1.000000000000000000 ) ) ;
#1533 = CARTESIAN_POINT ( 'NONE',  ( 2.061999999999999833, 0.000000000000000000, -1.812000000000000277 ) ) ;
#1534 = VERTEX_POINT ( 'NONE', #7652 ) ;
#1535 = DIRECTION ( 'NONE',  ( -1.000000000000000000, -0.000000000000000000, -0.000000000000000000 ) ) ;
#1536 = ORIENTED_EDGE ( 'NONE', *, *, #9240, .T. ) ;
#1537 = CARTESIAN_POINT ( 'NONE',  ( 0.7174986153957899626, -0.008289224748913706642, 0.4612806347796405415 ) ) ;
#1538 = ORIENTED_EDGE ( 'NONE', *, *, #4649, .T. ) ;
#1539 = CARTESIAN_POINT ( 'NONE',  ( 2.774999999999999911, -1.679378605318059048, -1.384878605318056399 ) ) ;
#1540 = AXIS2_PLACEMENT_3D ( 'NONE', #4462, #11418, #12785 ) ;
#1541 = DIRECTION ( 'NONE',  ( 1.000000000000000000, 0.000000000000000000, 0.000000000000000000 ) ) ;
#1542 = VECTOR ( 'NONE', #11886, 39.37007874015748143 ) ;
#1543 = CARTESIAN_POINT ( 'NONE',  ( 3.875000000000000000, 3.137999999999999901, 0.000000000000000000 ) ) ;
#1544 = LINE ( 'NONE', #6086, #671 ) ;
#1545 = CARTESIAN_POINT ( 'NONE',  ( 6.096491571325181269, 0.000000000000000000, 1.500000000000000222 ) ) ;
#1546 = ORIENTED_EDGE ( 'NONE', *, *, #12964, .F. ) ;
#1547 = ORIENTED_EDGE ( 'NONE', *, *, #8313, .F. ) ;
#1548 = ADVANCED_FACE ( 'NONE', ( #2215 ), #3879, .F. ) ;
#1549 = ORIENTED_EDGE ( 'NONE', *, *, #6080, .T. ) ;
#1550 = VECTOR ( 'NONE', #10497, 39.37007874015748143 ) ;
#1551 = EDGE_CURVE ( 'NONE', #8873, #13688, #3386, .T. ) ;
#1552 = DIRECTION ( 'NONE',  ( -1.000000000000000000, -0.000000000000000000, -0.000000000000000000 ) ) ;
#1553 = EDGE_CURVE ( 'NONE', #5216, #7690, #5824, .T. ) ;
#1554 = CARTESIAN_POINT ( 'NONE',  ( 2.774999999999999911, -1.575000000000016387, -2.359999999999999876 ) ) ;
#1555 = DIRECTION ( 'NONE',  ( 0.000000000000000000, 1.000000000000000000, -0.000000000000000000 ) ) ;
#1556 = FACE_OUTER_BOUND ( 'NONE', #14489, .T. ) ;
#1557 = EDGE_CURVE ( 'NONE', #5573, #10807, #10487, .T. ) ;
#1558 = APPLICATION_CONTEXT ( 'automotive_design' ) ;
#1559 = FACE_OUTER_BOUND ( 'NONE', #14733, .T. ) ;
#1560 =( NAMED_UNIT ( * ) PLANE_ANGLE_UNIT ( ) SI_UNIT ( $, .RADIAN. ) );
#1561 = ORIENTED_EDGE ( 'NONE', *, *, #9832, .T. ) ;
#1562 = VERTEX_POINT ( 'NONE', #11552 ) ;
#1563 = EDGE_LOOP ( 'NONE', ( #10739, #7868, #1, #12847 ) ) ;
#1564 = FACE_OUTER_BOUND ( 'NONE', #4686, .T. ) ;
#1565 = DIMENSIONAL_EXPONENTS ( 1.000000000000000000, 0.000000000000000000, 0.000000000000000000, 0.000000000000000000, 0.000000000000000000, 0.000000000000000000, 0.000000000000000000 ) ;
#1566 = CONICAL_SURFACE ( 'NONE', #2319, 1.000000000000000000, 0.7853981633974488341 ) ;
#1567 = VECTOR ( 'NONE', #10993, 39.37007874015748854 ) ;
#1568 = CARTESIAN_POINT ( 'NONE',  ( -0.4424999999999982836, -0.6590000000000000302, 0.3724999999999999423 ) ) ;
#1569 = PLANE ( 'NONE',  #5999 ) ;
#1570 = CARTESIAN_POINT ( 'NONE',  ( 2.957700166089386240, 0.9550922613677920170, 0.4582245739251649685 ) ) ;
#1571 = ORIENTED_EDGE ( 'NONE', *, *, #3241, .F. ) ;
#1572 =( BOUNDED_SURFACE ( )  B_SPLINE_SURFACE ( 3, 2, ( 
 ( #2820, #8706, #13352 ),
 ( #9573, #3966, #495 ),
 ( #2894, #12149, #12003 ),
 ( #12072, #7490, #14217 ),
 ( #2679, #13209, #5190 ),
 ( #7350, #7276, #11929 ),
 ( #1510, #14290, #1440 ),
 ( #6129, #10787, #275 ),
 ( #4978, #9644, #3828 ),
 ( #349, #8497, #10856 ),
 ( #5052, #9716, #14364 ),
 ( #3901, #2746, #1584 ),
 ( #6273, #10932, #424 ),
 ( #5127, #9783, #14439 ),
 ( #6573, #10019, #7711 ),
 ( #14673, #14745, #7629 ),
 ( #3270, #3199, #1726 ),
 ( #13501, #10239, #8789 ),
 ( #5570, #7862, #13433 ),
 ( #3126, #647, #11230 ),
 ( #2030, #10162, #7792 ),
 ( #5346, #4271, #14898 ),
 ( #9089, #4199, #13732 ),
 ( #14818, #727, #5423 ),
 ( #11069, #4121, #9934 ),
 ( #4347, #8863, #10090 ),
 ( #5495, #12369, #12512 ),
 ( #6716, #11378, #5263 ),
 ( #9022, #567, #13664 ),
 ( #3041, #13582, #8939 ),
 ( #7937, #876, #1883 ),
 ( #1802, #14588, #12445 ),
 ( #4424, #6413, #1962 ),
 ( #6645, #11298, #797 ),
 ( #2969, #12289, #6492 ),
 ( #11149, #8261, #10310 ),
 ( #8101, #3345, #12588 ),
 ( #2436, #2111, #106 ),
 ( #11765, #5723, #10461 ),
 ( #12741, #14123, #14041 ),
 ( #15050, #9246, #5948 ),
 ( #5800, #2267, #11607 ),
 ( #13961, #11532, #6951 ),
 ( #12898, #5883, #3496 ),
 ( #12671, #7115, #1263 ),
 ( #2350, #14970, #3663 ),
 ( #3581, #8022, #1113 ),
 ( #4496, #2194, #8177 ),
 ( #6879, #10539, #15126 ),
 ( #6796, #1192, #11458 ),
 ( #10611, #4807, #33 ),
 ( #4726, #959, #9400 ),
 ( #9166, #9476, #12818 ),
 ( #13810, #1033, #4652 ),
 ( #9322, #10385, #4575 ),
 ( #7032, #11691, #2503 ),
 ( #4889, #402, #12130 ),
 ( #8475, #9553, #13191 ),
 ( #9834, #14197, #1492 ),
 ( #9765, #2579, #10834 ),
 ( #7256, #326, #1636 ),
 ( #6328, #6110, #10986 ),
 ( #475, #1709, #10069 ),
 ( #8843, #14801, #7769 ),
 ( #4255, #7689, #7846 ),
 ( #12493, #779, #11051 ),
 ( #2014, #8917, #9913 ),
 ( #1947, #14569, #11515 ),
 ( #5864, #8242, #10367 ),
 ( #12648, #2252, #2411 ),
 ( #7918, #2176, #4558 ),
 ( #9306, #1092, #9225 ),
 ( #5705, #13789, #1015 ),
 ( #4409, #14881, #9382 ),
 ( #13944, #9070, #13863 ),
 ( #5635, #3559, #8084 ),
 ( #6932, #10445, #11588 ),
 ( #1245, #7999, #13716 ),
 ( #8159, #3250, #7096 ),
 ( #12799, #11435, #2330 ),
 ( #7014, #941, #14953 ),
 ( #11667, #10521, #18 ),
 ( #5918, #14166, #10426 ),
 ( #14004, #3538, #3621 ),
 ( #10656, #2470, #5990 ),
 ( #3390, #9519, #7152 ),
 ( #11802, #1152, #2235 ),
 ( #10576, #2310, #1379 ) ),
 .UNSPECIFIED., .F., .F., .F. ) 
 B_SPLINE_SURFACE_WITH_KNOTS ( ( 4, 2, 2, 2, 2, 2, 2, 2, 2, 2, 2, 2, 2, 2, 2, 2, 2, 2, 2, 2, 2, 2, 2, 2, 2, 2, 2, 2, 2, 2, 2, 2, 2, 2, 2, 2, 2, 2, 2, 2, 2, 2, 2, 4 ),
 ( 3, 3 ),
 ( 0.02004080291861797675, 0.02305506901397080116, 0.02606933510932362211, 0.02757646815700003085, 0.02908360120467644305, 0.03209786730002926747, 0.03360500034770567968, 0.03511213339538209188, 0.03812639949073490936, 0.04114066558608772683, 0.04415493168144055125, 0.04716919777679337566, 0.04867633082446978787, 0.05018346387214620008, 0.05319772996749902449, 0.05470486301517543670, 0.05621199606285184197, 0.05922626215820465945, 0.06224052825355748386, 0.06374766130123389607, 0.06525479434891030828, 0.06826906044426313269, 0.06977619349193953102, 0.07128332653961594323, 0.07429759263496876764, 0.07731185873032159206, 0.07881899177799800427, 0.08032612482567441647, 0.08334039092102724089, 0.08635465701638006530, 0.08936892311173288972, 0.09087605615940930193, 0.09238318920708571413, 0.09539745530243853855, 0.09841172139779136296, 0.09991885444546777517, 0.1014259874931441874, 0.1044402535884970118, 0.1059473866361734240, 0.1074545196838498362, 0.1104687857792026606, 0.1119759188268790728, 0.1134830518745554850, 0.1164973179699082956 ),
 ( 0.000000000000000000, 1.000000000000000000 ),
 .UNSPECIFIED. ) 
 GEOMETRIC_REPRESENTATION_ITEM ( )  RATIONAL_B_SPLINE_SURFACE ( (
 ( 1.000000000000000000, 0.7303619642676426604, 1.000000000000000000),
 ( 1.000000000000000000, 0.7391659050363718064, 1.000000000000000000),
 ( 1.000000000000000000, 0.7477864703932980417, 1.000000000000000000),
 ( 1.000000000000000000, 0.7644820136340396699, 1.000000000000000000),
 ( 1.000000000000000000, 0.7725576652621481966, 1.000000000000000000),
 ( 1.000000000000000000, 0.7841369972240639363, 1.000000000000000000),
 ( 1.000000000000000000, 0.7879067894510097814, 1.000000000000000000),
 ( 1.000000000000000000, 0.7951473863334842518, 1.000000000000000000),
 ( 1.000000000000000000, 0.7986319938952645137, 1.000000000000000000),
 ( 1.000000000000000000, 0.8086632967091734736, 1.000000000000000000),
 ( 1.000000000000000000, 0.8147886344311031648, 1.000000000000000000),
 ( 1.000000000000000000, 0.8230549922231803484, 1.000000000000000000),
 ( 1.000000000000000000, 0.8256565766521759553, 1.000000000000000000),
 ( 1.000000000000000000, 0.8305349661893675073, 1.000000000000000000),
 ( 1.000000000000000000, 0.8328179003807386627, 1.000000000000000000),
 ( 1.000000000000000000, 0.8391074215019772575, 1.000000000000000000),
 ( 1.000000000000000000, 0.8424994775394850643, 1.000000000000000000),
 ( 1.000000000000000000, 0.8477154134529806262, 1.000000000000000000),
 ( 1.000000000000000000, 0.8495388365352557480, 1.000000000000000000),
 ( 1.000000000000000000, 0.8516216512933566518, 1.000000000000000000),
 ( 1.000000000000000000, 0.8518656269916470292, 1.000000000000000000),
 ( 1.000000000000000000, 0.8508610807012660926, 1.000000000000000000),
 ( 1.000000000000000000, 0.8496312072233146440, 1.000000000000000000),
 ( 1.000000000000000000, 0.8468793023704244138, 1.000000000000000000),
 ( 1.000000000000000000, 0.8458107531247578414, 1.000000000000000000),
 ( 1.000000000000000000, 0.8434028339490304838, 1.000000000000000000),
 ( 1.000000000000000000, 0.8420586255985930135, 1.000000000000000000),
 ( 1.000000000000000000, 0.8377450007014299871, 1.000000000000000000),
 ( 1.000000000000000000, 0.8344806938985878109, 1.000000000000000000),
 ( 1.000000000000000000, 0.8292948692869647198, 1.000000000000000000),
 ( 1.000000000000000000, 0.8275179307216389279, 1.000000000000000000),
 ( 1.000000000000000000, 0.8239169748456836029, 1.000000000000000000),
 ( 1.000000000000000000, 0.8220876319902808982, 1.000000000000000000),
 ( 1.000000000000000000, 0.8166433934471487577, 1.000000000000000000),
 ( 1.000000000000000000, 0.8131103617266270955, 1.000000000000000000),
 ( 1.000000000000000000, 0.8066241410163590420, 1.000000000000000000),
 ( 1.000000000000000000, 0.8036703286668861468, 1.000000000000000000),
 ( 1.000000000000000000, 0.7999468164656692304, 1.000000000000000000),
 ( 1.000000000000000000, 0.7988220075153393829, 1.000000000000000000),
 ( 1.000000000000000000, 0.7968807107365607489, 1.000000000000000000),
 ( 1.000000000000000000, 0.7960588307793206031, 1.000000000000000000),
 ( 1.000000000000000000, 0.7940666135324694341, 1.000000000000000000),
 ( 1.000000000000000000, 0.7933721712197883136, 1.000000000000000000),
 ( 1.000000000000000000, 0.7933444941328147149, 1.000000000000000000),
 ( 1.000000000000000000, 0.7935036486169138037, 1.000000000000000000),
 ( 1.000000000000000000, 0.7941617368941129573, 1.000000000000000000),
 ( 1.000000000000000000, 0.7946641558677889350, 1.000000000000000000),
 ( 1.000000000000000000, 0.7966418117377881414, 1.000000000000000000),
 ( 1.000000000000000000, 0.7985862221323072330, 1.000000000000000000),
 ( 1.000000000000000000, 0.8034606050232417918, 1.000000000000000000),
 ( 1.000000000000000000, 0.8063907621180180785, 1.000000000000000000),
 ( 1.000000000000000000, 0.8112888969071575529, 1.000000000000000000),
 ( 1.000000000000000000, 0.8130019067800049459, 1.000000000000000000),
 ( 1.000000000000000000, 0.8164902207451381067, 1.000000000000000000),
 ( 1.000000000000000000, 0.8182717664989170858, 1.000000000000000000),
 ( 1.000000000000000000, 0.8236513966877028192, 1.000000000000000000),
 ( 1.000000000000000000, 0.8272847376777223705, 1.000000000000000000),
 ( 1.000000000000000000, 0.8342391892289522382, 1.000000000000000000),
 ( 1.000000000000000000, 0.8375729779648963813, 1.000000000000000000),
 ( 1.000000000000000000, 0.8433263320323867163, 1.000000000000000000),
 ( 1.000000000000000000, 0.8457747513117915839, 1.000000000000000000),
 ( 1.000000000000000000, 0.8485728704767122599, 1.000000000000000000),
 ( 1.000000000000000000, 0.8493599451720096338, 1.000000000000000000),
 ( 1.000000000000000000, 0.8506036242994673424, 1.000000000000000000),
 ( 1.000000000000000000, 0.8510608768027098092, 1.000000000000000000),
 ( 1.000000000000000000, 0.8518668280105339274, 1.000000000000000000),
 ( 1.000000000000000000, 0.8516595178598228566, 1.000000000000000000),
 ( 1.000000000000000000, 0.8496680361726848263, 1.000000000000000000),
 ( 1.000000000000000000, 0.8478847233904961422, 1.000000000000000000),
 ( 1.000000000000000000, 0.8439514783278239118, 1.000000000000000000),
 ( 1.000000000000000000, 0.8424398969624482536, 1.000000000000000000),
 ( 1.000000000000000000, 0.8390475808887900566, 1.000000000000000000),
 ( 1.000000000000000000, 0.8371639927170544393, 1.000000000000000000),
 ( 1.000000000000000000, 0.8309672570077345499, 1.000000000000000000),
 ( 1.000000000000000000, 0.8261093469114791921, 1.000000000000000000),
 ( 1.000000000000000000, 0.8177745008309323937, 1.000000000000000000),
 ( 1.000000000000000000, 0.8148147276102298830, 1.000000000000000000),
 ( 1.000000000000000000, 0.8086351537547810109, 1.000000000000000000),
 ( 1.000000000000000000, 0.8054072265268824582, 1.000000000000000000),
 ( 1.000000000000000000, 0.7953363259039076816, 1.000000000000000000),
 ( 1.000000000000000000, 0.7881068092093646005, 1.000000000000000000),
 ( 1.000000000000000000, 0.7765812923454467054, 1.000000000000000000),
 ( 1.000000000000000000, 0.7726257270913668984, 1.000000000000000000),
 ( 1.000000000000000000, 0.7645013318077583664, 1.000000000000000000),
 ( 1.000000000000000000, 0.7603508406709547085, 1.000000000000000000),
 ( 1.000000000000000000, 0.7477573469669197559, 1.000000000000000000),
 ( 1.000000000000000000, 0.7391362403695903582, 1.000000000000000000),
 ( 1.000000000000000000, 0.7303873157140532424, 1.000000000000000000) ) ) 
 REPRESENTATION_ITEM ( '' )  SURFACE ( )  );
#1573 = DIRECTION ( 'NONE',  ( 0.000000000000000000, 0.000000000000000000, 1.000000000000000000 ) ) ;
#1574 = CARTESIAN_POINT ( 'NONE',  ( 3.379935043499636027, 2.435578798916048893, 0.5650223589646659050 ) ) ;
#1575 = DIRECTION ( 'NONE',  ( 0.000000000000000000, 1.000000000000000000, -4.591341165821855765E-15 ) ) ;
#1576 = CARTESIAN_POINT ( 'NONE',  ( 6.826491571325181695, 0.000000000000000000, 3.000000000000000444 ) ) ;
#1577 = EDGE_CURVE ( 'NONE', #15129, #2976, #12694, .T. ) ;
#1578 = AXIS2_PLACEMENT_3D ( 'NONE', #12455, #8949, #13897 ) ;
#1579 = CARTESIAN_POINT ( 'NONE',  ( 3.426491571325181340, -1.574999999999999956, 2.360000000000024745 ) ) ;
#1580 = VECTOR ( 'NONE', #11310, 39.37007874015748143 ) ;
#1581 = CARTESIAN_POINT ( 'NONE',  ( 2.774999999999999911, 1.679378605318042395, -1.384878605318059952 ) ) ;
#1582 = EDGE_CURVE ( 'NONE', #12204, #11537, #15071, .T. ) ;
#1583 = DIRECTION ( 'NONE',  ( 1.000000000000000000, 0.000000000000000000, 0.000000000000000000 ) ) ;
#1584 = CARTESIAN_POINT ( 'NONE',  ( 3.760602986904977740, 1.815251021643483176, 0.7937676298150420084 ) ) ;
#1585 = CARTESIAN_POINT ( 'NONE',  ( 6.826491571325181695, 0.000000000000000000, 2.960629921259841257 ) ) ;
#1586 = ORIENTED_EDGE ( 'NONE', *, *, #6661, .F. ) ;
#1587 = CARTESIAN_POINT ( 'NONE',  ( 2.774999999999999911, 0.9800000000000039790, 2.359999999999999876 ) ) ;
#1589 = ORIENTED_EDGE ( 'NONE', *, *, #10671, .T. ) ;
#1588 = CARTESIAN_POINT ( 'NONE',  ( 3.426491571325181340, 0.000000000000000000, 0.000000000000000000 ) ) ;
#1590 = ORIENTED_EDGE ( 'NONE', *, *, #12794, .F. ) ;
#1591 = CARTESIAN_POINT ( 'NONE',  ( -0.4424999999999985612, -0.6590000000000000302, -0.8499999999999999778 ) ) ;
#1592 = CARTESIAN_POINT ( 'NONE',  ( 0.8999999999999999112, -0.6230000000000016636, -0.3750000000000000555 ) ) ;
#1593 = VERTEX_POINT ( 'NONE', #9270 ) ;
#1594 = DIRECTION ( 'NONE',  ( -0.7071067811865436870, 0.000000000000000000, 0.7071067811865512365 ) ) ;
#1595 = AXIS2_PLACEMENT_3D ( 'NONE', #14987, #6822, #12758 ) ;
#1596 = DIRECTION ( 'NONE',  ( -1.000000000000000000, -0.000000000000000000, -0.000000000000000000 ) ) ;
#1597 = CARTESIAN_POINT ( 'NONE',  ( -0.3725000000000002198, -0.6590000000000000302, -0.4125000000000000333 ) ) ;
#1598 = EDGE_LOOP ( 'NONE', ( #987, #1622, #1219, #6590 ) ) ;
#1599 = ADVANCED_FACE ( 'NONE', ( #15147, #6972 ), #8120, .T. ) ;
#1600 = SHAPE_REPRESENTATION ( 'Hex Bolt', ( #8424 ), #10848 ) ;
#1601 = CARTESIAN_POINT ( 'NONE',  ( 0.1250000000000009992, 1.224646799147353207E-16, -1.000000000000000000 ) ) ;
#1602 = LINE ( 'NONE', #13085, #12748 ) ;
#1603 = AXIS2_PLACEMENT_3D ( 'NONE', #11666, #5862, #10520 ) ;
#1604 = PLANE ( 'NONE',  #5846 ) ;
#1605 = CIRCLE ( 'NONE', #10179, 0.2219999999999999751 ) ;
#1606 = VERTEX_POINT ( 'NONE', #12840 ) ;
#1607 = DIRECTION ( 'NONE',  ( -0.7070715176384831935, -0.7070715176384805289, -0.009986885842351451645 ) ) ;
#1608 = EDGE_LOOP ( 'NONE', ( #5201, #5091, #11749, #7779 ) ) ;
#1609 = ORIENTED_EDGE ( 'NONE', *, *, #13267, .F. ) ;
#1610 = CARTESIAN_POINT ( 'NONE',  ( 0.06299999999999994493, -1.679378605318048390, 1.679378605318054163 ) ) ;
#1611 = AXIS2_PLACEMENT_3D ( 'NONE', #10243, #11382, #12675 ) ;
#1612 = FACE_OUTER_BOUND ( 'NONE', #1246, .T. ) ;
#1613 = CARTESIAN_POINT ( 'NONE',  ( 5.103871432852032264, 3.303028361439904081, 0.3679054358681541625 ) ) ;
#1614 = AXIS2_PLACEMENT_3D ( 'NONE', #12574, #13489, #6634 ) ;
#1615 = LINE ( 'NONE', #2634, #8299 ) ;
#1616 = CYLINDRICAL_SURFACE ( 'NONE', #12564, 0.4349999999999999423 ) ;
#1617 = ADVANCED_FACE ( 'NONE', ( #3446 ), #7051, .F. ) ;
#1618 = CARTESIAN_POINT ( 'NONE',  ( 0.06299999999999998657, 0.000000000000000000, -1.875500000000000167 ) ) ;
#1619 = CONICAL_SURFACE ( 'NONE', #5792, 0.06999999999999829969, 0.7853981633974298493 ) ;
#1620 = ORIENTED_EDGE ( 'NONE', *, *, #1918, .F. ) ;
#1621 = ORIENTED_EDGE ( 'NONE', *, *, #5490, .F. ) ;
#1622 = ORIENTED_EDGE ( 'NONE', *, *, #5988, .F. ) ;
#1623 = CARTESIAN_POINT ( 'NONE',  ( 2.124999999999999556, -1.679378605318041950, 1.679378605318059048 ) ) ;
#1624 = DIRECTION ( 'NONE',  ( 0.000000000000000000, 0.000000000000000000, -1.000000000000000000 ) ) ;
#1625 = CIRCLE ( 'NONE', #10929, 2.500000000000000444 ) ;
#1626 = CARTESIAN_POINT ( 'NONE',  ( 4.344846310392954436, 3.567999999999999616, -1.491010071662831171 ) ) ;
#1627 = DIRECTION ( 'NONE',  ( 1.000000000000000000, 0.000000000000000000, 0.000000000000000000 ) ) ;
#1628 = PRODUCT_DEFINITION_SHAPE ( 'NONE', 'NONE',  #3599 ) ;
#1629 = CYLINDRICAL_SURFACE ( 'NONE', #5363, 0.3750000000000004996 ) ;
#1630 = CARTESIAN_POINT ( 'NONE',  ( 3.971130012676523879, 1.827282607391995883, 0.7455485334240098405 ) ) ;
#1631 = EDGE_CURVE ( 'NONE', #1935, #9095, #11631, .T. ) ;
#1632 = EDGE_CURVE ( 'NONE', #7301, #7267, #12420, .T. ) ;
#1633 = ADVANCED_FACE ( 'NONE', ( #10328 ), #4000, .T. ) ;
#1634 = CARTESIAN_POINT ( 'NONE',  ( 0.000000000000000000, 0.000000000000000000, 0.000000000000000000 ) ) ;
#1635 = CIRCLE ( 'NONE', #10211, 0.2624999999999997335 ) ;
#1636 = CARTESIAN_POINT ( 'NONE',  ( 4.335720917399813246, 1.707353294205550487, -0.6508460809909353273 ) ) ;
#1637 = ORIENTED_EDGE ( 'NONE', *, *, #6722, .T. ) ;
#1638 = ORIENTED_EDGE ( 'NONE', *, *, #14739, .T. ) ;
#1639 = EDGE_CURVE ( 'NONE', #14903, #5034, #6305, .T. ) ;
#1640 = EDGE_LOOP ( 'NONE', ( #9824, #615, #14579, #12098 ) ) ;
#1641 = CARTESIAN_POINT ( 'NONE',  ( 6.787121492585022509, 0.000000000000000000, 1.000000000000000000 ) ) ;
#1642 = LINE ( 'NONE', #13339, #6042 ) ;
#1644 = AXIS2_PLACEMENT_3D ( 'NONE', #2005, #3182, #10362 ) ;
#1643 = DIRECTION ( 'NONE',  ( -1.000000000000000000, -0.000000000000000000, -0.000000000000000000 ) ) ;
#1645 = CARTESIAN_POINT ( 'NONE',  ( 3.874999999999999556, 3.567999999999999616, -1.320000000000000062 ) ) ;
#1646 = ORIENTED_EDGE ( 'NONE', *, *, #1413, .F. ) ;
#1647 = DIRECTION ( 'NONE',  ( 0.000000000000000000, 0.000000000000000000, 1.000000000000000000 ) ) ;
#1648 = CARTESIAN_POINT ( 'NONE',  ( 2.774999999999999911, 0.000000000000000000, 0.000000000000000000 ) ) ;
#1649 = VECTOR ( 'NONE', #7357, 39.37007874015748143 ) ;
#1650 = CARTESIAN_POINT ( 'NONE',  ( 3.426491571325181340, 3.137999999999999901, 0.2209981660730358233 ) ) ;
#1651 = EDGE_CURVE ( 'NONE', #1686, #13105, #2712, .T. ) ;
#1652 = VECTOR ( 'NONE', #3367, 39.37007874015748854 ) ;
#1653 = CIRCLE ( 'NONE', #10223, 0.8499999999999999778 ) ;
#1654 = DIRECTION ( 'NONE',  ( -0.4671160445299247232, 0.000000000000000000, 0.8841960195243572240 ) ) ;
#1655 = VECTOR ( 'NONE', #4137, 39.37007874015748143 ) ;
#1656 = CARTESIAN_POINT ( 'NONE',  ( 0.8336852985356730805, -0.4829999999999999294, -0.4100337033397443709 ) ) ;
#1657 = DIRECTION ( 'NONE',  ( -0.7071067811865447972, 0.000000000000000000, 0.7071067811865501263 ) ) ;
#1659 = ORIENTED_EDGE ( 'NONE', *, *, #9256, .T. ) ;
#1658 = DIRECTION ( 'NONE',  ( 0.000000000000000000, 0.000000000000000000, -1.000000000000000000 ) ) ;
#1660 = ORIENTED_EDGE ( 'NONE', *, *, #5029, .T. ) ;
#1661 = CARTESIAN_POINT ( 'NONE',  ( 3.426491571325180452, 1.978105636280900193, 0.6428442102750744347 ) ) ;
#1663 = ORIENTED_EDGE ( 'NONE', *, *, #13541, .T. ) ;
#1662 = DIRECTION ( 'NONE',  ( -1.000000000000000000, -0.000000000000000000, -0.000000000000000000 ) ) ;
#1664 = VECTOR ( 'NONE', #9359, 39.37007874015748143 ) ;
#1665 = ORIENTED_EDGE ( 'NONE', *, *, #10203, .T. ) ;
#1666 = CIRCLE ( 'NONE', #11947, 0.2219999999999999751 ) ;
#1667 = EDGE_CURVE ( 'NONE', #6474, #13739, #8757, .T. ) ;
#1668 = CARTESIAN_POINT ( 'NONE',  ( 2.567289415621050175, 0.8512991579513188301, -0.4032946756736221494 ) ) ;
#1669 =( LENGTH_UNIT ( ) NAMED_UNIT ( * ) SI_UNIT ( $, .METRE. ) );
#1670 = DIRECTION ( 'NONE',  ( -1.000000000000000000, -0.000000000000000000, -0.000000000000000000 ) ) ;
#1671 = ORIENTED_EDGE ( 'NONE', *, *, #12242, .F. ) ;
#1672 = AXIS2_PLACEMENT_3D ( 'NONE', #10806, #11954, #4850 ) ;
#1673 = LINE ( 'NONE', #7500, #7464 ) ;
#1674 = FACE_OUTER_BOUND ( 'NONE', #2096, .T. ) ;
#1675 = AXIS2_PLACEMENT_3D ( 'NONE', #14282, #8275, #340 ) ;
#1676 = EDGE_CURVE ( 'NONE', #13657, #34, #1416, .T. ) ;
#1677 = CIRCLE ( 'NONE', #2675, 0.03999999999999998002 ) ;
#1678 = CARTESIAN_POINT ( 'NONE',  ( 0.7429783265673484127, 2.717297069309015269E-16, 0.4366554833170019356 ) ) ;
#1679 = CARTESIAN_POINT ( 'NONE',  ( -0.7287617923574205570, 0.2159999999999999420, -0.4425000000000005596 ) ) ;
#1680 = ORIENTED_EDGE ( 'NONE', *, *, #9849, .T. ) ;
#1681 = DIRECTION ( 'NONE',  ( 0.000000000000000000, 0.000000000000000000, -1.000000000000000000 ) ) ;
#1682 = MECHANICAL_DESIGN_GEOMETRIC_PRESENTATION_REPRESENTATION (  '', ( #13406 ), #9532 ) ;
#1683 = CARTESIAN_POINT ( 'NONE',  ( 0.2249147617188371751, 1.239999999999999991, -0.3723417112827391295 ) ) ;
#1684 = CARTESIAN_POINT ( 'NONE',  ( 2.775039370078740131, 1.679378605318035733, -2.054378605318066153 ) ) ;
#1685 = SURFACE_STYLE_FILL_AREA ( #9878 ) ;
#1686 = VERTEX_POINT ( 'NONE', #7519 ) ;
#1687 = AXIS2_PLACEMENT_3D ( 'NONE', #5024, #9690, #3492 ) ;
#1688 = CYLINDRICAL_SURFACE ( 'NONE', #8701, 0.2624999999999852451 ) ;
#1689 = EDGE_LOOP ( 'NONE', ( #11701, #2417, #13648, #11639 ) ) ;
#1690 = CARTESIAN_POINT ( 'NONE',  ( 1.250000000000000000, 0.000000000000000000, 0.4223386481965726857 ) ) ;
#1691 = VERTEX_POINT ( 'NONE', #6159 ) ;
#1692 = DIRECTION ( 'NONE',  ( -0.000000000000000000, -1.000000000000000000, -0.000000000000000000 ) ) ;
#1693 = EDGE_CURVE ( 'NONE', #2057, #4509, #3636, .T. ) ;
#1694 = EDGE_CURVE ( 'NONE', #5675, #13385, #10717, .T. ) ;
#1695 = LINE ( 'NONE', #6156, #6855 ) ;
#1696 = VECTOR ( 'NONE', #14543, 39.37007874015748143 ) ;
#1697 = CARTESIAN_POINT ( 'NONE',  ( 6.794491571325179891, -1.679378605318047946, -1.679378605318053497 ) ) ;
#1698 = CARTESIAN_POINT ( 'NONE',  ( 0.06299999999999994493, 1.679378605318059492, 1.679378605318041506 ) ) ;
#1699 = LINE ( 'NONE', #10894, #8923 ) ;
#1700 = CARTESIAN_POINT ( 'NONE',  ( 1.250847373107695670, -0.05999999999999990757, -0.4823326642216427818 ) ) ;
#1701 = ORIENTED_EDGE ( 'NONE', *, *, #8504, .F. ) ;
#1702 = ORIENTED_EDGE ( 'NONE', *, *, #6076, .T. ) ;
#1703 = VERTEX_POINT ( 'NONE', #7313 ) ;
#1704 = FACE_OUTER_BOUND ( 'NONE', #5355, .T. ) ;
#1705 = ORIENTED_EDGE ( 'NONE', *, *, #1693, .T. ) ;
#1706 = DIRECTION ( 'NONE',  ( 0.000000000000000000, 0.000000000000000000, -1.000000000000000000 ) ) ;
#1707 = CARTESIAN_POINT ( 'NONE',  ( 6.826491571325181695, 0.000000000000000000, 0.000000000000000000 ) ) ;
#1708 = CARTESIAN_POINT ( 'NONE',  ( 4.586453973344011281, 1.802653555183125755, 0.2432409261222566454 ) ) ;
#1709 = CARTESIAN_POINT ( 'NONE',  ( 4.247411616490353481, 1.732648565181565070, -0.6521631700520624797 ) ) ;
#1710 = ORIENTED_EDGE ( 'NONE', *, *, #11233, .F. ) ;
#1711 = ORIENTED_EDGE ( 'NONE', *, *, #12290, .T. ) ;
#1712 = ORIENTED_EDGE ( 'NONE', *, *, #10067, .T. ) ;
#1713 = DIRECTION ( 'NONE',  ( 0.9999002670844990837, 1.110054405283695815E-35, -0.01412288512831213171 ) ) ;
#1714 = EDGE_CURVE ( 'NONE', #5032, #1043, #1544, .T. ) ;
#1715 = DIRECTION ( 'NONE',  ( 0.000000000000000000, 0.000000000000000000, -1.000000000000000000 ) ) ;
#1716 = CYLINDRICAL_SURFACE ( 'NONE', #2584, 0.2625000000000000111 ) ;
#1717 = CONTEXT_DEPENDENT_SHAPE_REPRESENTATION ( #7349, #1384 ) ;
#1718 = CARTESIAN_POINT ( 'NONE',  ( 3.339621231360053955, 1.044107824239231430, 0.3927132934522771790 ) ) ;
#1719 = VERTEX_POINT ( 'NONE', #8603 ) ;
#1720 = DIRECTION ( 'NONE',  ( -0.9702019082525985549, 0.2422978687958610433, 0.000000000000000000 ) ) ;
#1721 = FACE_OUTER_BOUND ( 'NONE', #9981, .T. ) ;
#1722 = CARTESIAN_POINT ( 'NONE',  ( 8.474190026735612946, 0.9969999999999998863, 0.3203020658980471613 ) ) ;
#1723 = AXIS2_PLACEMENT_3D ( 'NONE', #3877, #8553, #2729 ) ;
#1724 = CARTESIAN_POINT ( 'NONE',  ( 0.4124999999999999223, -0.6290000000000003366, 0.3724999999999999423 ) ) ;
#1725 = CARTESIAN_POINT ( 'NONE',  ( 0.9301956387621866940, -0.4439432733257490660, -0.4442820374925280369 ) ) ;
#1726 = CARTESIAN_POINT ( 'NONE',  ( 3.931979536481067683, 1.764175763689243670, 0.7956254023616837756 ) ) ;
#1728 = ORIENTED_EDGE ( 'NONE', *, *, #14216, .F. ) ;
#1727 = DIRECTION ( 'NONE',  ( 0.000000000000000000, 0.000000000000000000, 1.000000000000000000 ) ) ;
#1729 = ORIENTED_EDGE ( 'NONE', *, *, #5239, .T. ) ;
#1730 = CARTESIAN_POINT ( 'NONE',  ( 0.6500000000000001332, -1.679378605318048390, 1.679378605318054163 ) ) ;
#1732 = ORIENTED_EDGE ( 'NONE', *, *, #11459, .T. ) ;
#1731 = DIRECTION ( 'NONE',  ( -1.000000000000000000, -0.000000000000000000, -0.000000000000000000 ) ) ;
#1733 = VERTEX_POINT ( 'NONE', #3863 ) ;
#1734 = EDGE_CURVE ( 'NONE', #937, #524, #2654, .T. ) ;
#1735 = CARTESIAN_POINT ( 'NONE',  ( 0.4349999999999999978, 1.239999999999999991, 0.000000000000000000 ) ) ;
#1736 = CARTESIAN_POINT ( 'NONE',  ( 0.000000000000000000, 5.750000000000000000, 0.000000000000000000 ) ) ;
#1737 = ORIENTED_EDGE ( 'NONE', *, *, #7176, .T. ) ;
#1738 = EDGE_CURVE ( 'NONE', #8382, #5425, #7069, .T. ) ;
#1739 = VECTOR ( 'NONE', #1939, 39.37007874015748143 ) ;
#1740 = DIRECTION ( 'NONE',  ( -2.602462600580851747E-17, -1.000000000000000000, 0.000000000000000000 ) ) ;
#1741 = FACE_OUTER_BOUND ( 'NONE', #2182, .T. ) ;
#1742 = CARTESIAN_POINT ( 'NONE',  ( 6.176491571325181340, 0.000000000000000000, -1.580000000000000071 ) ) ;
#1743 = EDGE_CURVE ( 'NONE', #2016, #10545, #8458, .T. ) ;
#1744 = LINE ( 'NONE', #11085, #6232 ) ;
#1745 = CARTESIAN_POINT ( 'NONE',  ( 0.000000000000000000, 0.000000000000000000, 0.000000000000000000 ) ) ;
#1746 = ADVANCED_FACE ( 'NONE', ( #386 ), #7384, .F. ) ;
#1747 = ORIENTED_EDGE ( 'NONE', *, *, #1011, .T. ) ;
#1748 = DIRECTION ( 'NONE',  ( -0.000000000000000000, -1.000000000000000000, -0.000000000000000000 ) ) ;
#1749 = DIRECTION ( 'NONE',  ( -0.000000000000000000, -1.000000000000000000, -0.000000000000000000 ) ) ;
#1750 = CYLINDRICAL_SURFACE ( 'NONE', #3389, 0.3750000000000004996 ) ;
#1751 = ORIENTED_EDGE ( 'NONE', *, *, #13636, .F. ) ;
#1752 = PRODUCT ( 'Ball Valve Sub', 'Ball Valve Sub', '', ( #6185 ) ) ;
#1753 = LINE ( 'NONE', #12393, #6996 ) ;
#1754 = DIRECTION ( 'NONE',  ( 0.000000000000000000, 0.000000000000000000, 1.000000000000000000 ) ) ;
#1755 = ORIENTED_EDGE ( 'NONE', *, *, #10453, .F. ) ;
#1756 = CARTESIAN_POINT ( 'NONE',  ( 3.426491571325181340, 2.426945040795776443, -0.5999481385559803925 ) ) ;
#1757 = ORIENTED_EDGE ( 'NONE', *, *, #10479, .T. ) ;
#1758 = FILL_AREA_STYLE_COLOUR ( '', #9999 ) ;
#1759 = AXIS2_PLACEMENT_3D ( 'NONE', #12410, #5537, #6612 ) ;
#1760 = CARTESIAN_POINT ( 'NONE',  ( 3.061616997868382402E-17, 1.109999999999999876, 0.2499999999999999167 ) ) ;
#1761 = DIRECTION ( 'NONE',  ( -0.000000000000000000, -0.000000000000000000, -1.000000000000000000 ) ) ;
#1762 = ADVANCED_FACE ( 'NONE', ( #13099 ), #9748, .T. ) ;
#1763 = CARTESIAN_POINT ( 'NONE',  ( 0.8268256298210439059, -0.4366477117775379169, -0.3581175243201347169 ) ) ;
#1764 = PLANE ( 'NONE',  #9015 ) ;
#1765 = EDGE_CURVE ( 'NONE', #788, #4442, #3784, .T. ) ;
#1766 = LINE ( 'NONE', #11109, #6231 ) ;
#1767 = CARTESIAN_POINT ( 'NONE',  ( 0.000000000000000000, 0.000000000000000000, 0.2041999999999996596 ) ) ;
#1768 = DIMENSIONAL_EXPONENTS ( 1.000000000000000000, 0.000000000000000000, 0.000000000000000000, 0.000000000000000000, 0.000000000000000000, 0.000000000000000000, 0.000000000000000000 ) ;
#1769 = EDGE_CURVE ( 'NONE', #12651, #10812, #1615, .T. ) ;
#1770 =( LENGTH_UNIT ( ) NAMED_UNIT ( * ) SI_UNIT ( $, .METRE. ) );
#1771 = CARTESIAN_POINT ( 'NONE',  ( 6.826491571325181695, -1.679378605318047946, -1.304378605318053053 ) ) ;
#1772 = VERTEX_POINT ( 'NONE', #461 ) ;
#1773 = VERTEX_POINT ( 'NONE', #1474 ) ;
#1774 = ORIENTED_EDGE ( 'NONE', *, *, #6348, .T. ) ;
#1775 = DIRECTION ( 'NONE',  ( 0.000000000000000000, 0.000000000000000000, -1.000000000000000000 ) ) ;
#1776 = VERTEX_POINT ( 'NONE', #8667 ) ;
#1777 = AXIS2_PLACEMENT_3D ( 'NONE', #1963, #8941, #14971 ) ;
#1778 = PLANE ( 'NONE',  #7685 ) ;
#1779 = CYLINDRICAL_SURFACE ( 'NONE', #23, 0.8000000000000000444 ) ;
#1780 = PLANE ( 'NONE',  #3898 ) ;
#1781 = CARTESIAN_POINT ( 'NONE',  ( 4.587994488202223664, 1.802825568755139996, -0.2425064940794559032 ) ) ;
#1782 = ORIENTED_EDGE ( 'NONE', *, *, #7638, .F. ) ;
#1783 = VECTOR ( 'NONE', #13825, 39.37007874015748143 ) ;
#1784 = VECTOR ( 'NONE', #158, 39.37007874015748143 ) ;
#1785 = EDGE_CURVE ( 'NONE', #8971, #5110, #305, .T. ) ;
#1786 = ORIENTED_EDGE ( 'NONE', *, *, #7425, .F. ) ;
#1787 = EDGE_LOOP ( 'NONE', ( #4413, #14242, #5193, #14105 ) ) ;
#1788 = ORIENTED_EDGE ( 'NONE', *, *, #12454, .T. ) ;
#1789 = LINE ( 'NONE', #4414, #6289 ) ;
#1790 = CARTESIAN_POINT ( 'NONE',  ( 0.8108060929038570785, -0.4829999999999998739, -0.3024090436974096185 ) ) ;
#1791 = DIRECTION ( 'NONE',  ( -0.000000000000000000, 1.000000000000000000, 0.000000000000000000 ) ) ;
#1792 = CARTESIAN_POINT ( 'NONE',  ( 3.475290612095096598, 0.9969999999995592388, 0.4509139744054365129 ) ) ;
#1793 = VERTEX_POINT ( 'NONE', #9818 ) ;
#1794 = CIRCLE ( 'NONE', #6695, 0.2624999999999852451 ) ;
#1795 = DIRECTION ( 'NONE',  ( 0.000000000000000000, 0.000000000000000000, 1.000000000000000000 ) ) ;
#1796 = CARTESIAN_POINT ( 'NONE',  ( 3.233755863391478247, 2.469910769216284940, 0.3874905525801941031 ) ) ;
#1797 = DIRECTION ( 'NONE',  ( -0.7071067811865422437, 0.000000000000000000, 0.7071067811865527908 ) ) ;
#1798 = CARTESIAN_POINT ( 'NONE',  ( 8.775135155112195662, 0.9377394161890534319, 0.2318982201004105848 ) ) ;
#1799 = CARTESIAN_POINT ( 'NONE',  ( 0.9149939388359350501, -0.4421793831954792808, -0.4489330281185069382 ) ) ;
#1800 = VECTOR ( 'NONE', #13513, 39.37007874015748854 ) ;
#1801 = EDGE_CURVE ( 'NONE', #7612, #14785, #12181, .T. ) ;
#1802 = CARTESIAN_POINT ( 'NONE',  ( 4.485621383300165022, 1.787868003613383161, 0.4380272511281654291 ) ) ;
#1804 = ORIENTED_EDGE ( 'NONE', *, *, #8532, .F. ) ;
#1803 = DIRECTION ( 'NONE',  ( 0.000000000000000000, 1.000000000000000000, 0.000000000000000000 ) ) ;
#1805 = ORIENTED_EDGE ( 'NONE', *, *, #13885, .F. ) ;
#1806 = CARTESIAN_POINT ( 'NONE',  ( -0.3208174396729924216, 1.603403006623433713, -0.2062334004842315271 ) ) ;
#1808 = VERTEX_POINT ( 'NONE', #12473 ) ;
#1807 = LINE ( 'NONE', #6496, #9692 ) ;
#1809 = EDGE_LOOP ( 'NONE', ( #12192, #14198, #4340, #6562 ) ) ;
#1810 = DIRECTION ( 'NONE',  ( 0.000000000000000000, -0.000000000000000000, -1.000000000000000000 ) ) ;
#1811 = CYLINDRICAL_SURFACE ( 'NONE', #3543, 0.4349999999999999423 ) ;
#1812 = ORIENTED_EDGE ( 'NONE', *, *, #11226, .T. ) ;
#1813 = CARTESIAN_POINT ( 'NONE',  ( 4.665325695584414469E-17, 1.603403463250997918, 0.3809527529760087239 ) ) ;
#1814 = DIRECTION ( 'NONE',  ( 0.8660254037844398178, 0.000000000000000000, 0.4999999999999980016 ) ) ;
#1815 = AXIS2_PLACEMENT_3D ( 'NONE', #1592, #3915, #10942 ) ;
#1816 = CARTESIAN_POINT ( 'NONE',  ( 3.426491571325181340, -1.679378605318059048, -1.679378605318041950 ) ) ;
#1817 = CIRCLE ( 'NONE', #12811, 0.8000000000000000444 ) ;
#1818 = AXIS2_PLACEMENT_3D ( 'NONE', #6677, #7746, #13765 ) ;
#1819 = CARTESIAN_POINT ( 'NONE',  ( 0.6734800455634090133, -0.02996288503340473197, 0.4827503109326272135 ) ) ;
#1820 = EDGE_CURVE ( 'NONE', #11264, #14935, #430, .T. ) ;
#1821 = CARTESIAN_POINT ( 'NONE',  ( 0.9745775721194528396, -0.4829504857673974083, -0.3850199534376020916 ) ) ;
#1822 = EDGE_CURVE ( 'NONE', #4605, #11449, #8981, .T. ) ;
#1823 = ORIENTED_EDGE ( 'NONE', *, *, #8555, .T. ) ;
#1824 = EDGE_CURVE ( 'NONE', #3063, #7156, #12254, .T. ) ;
#1825 = DIRECTION ( 'NONE',  ( -1.000000000000000000, 0.000000000000000000, 0.000000000000000000 ) ) ;
#1826 = CARTESIAN_POINT ( 'NONE',  ( 3.475375010813855248, 1.976875583815957071, 0.3014176176147594366 ) ) ;
#1827 = DIRECTION ( 'NONE',  ( 1.000000000000000000, 0.000000000000000000, 0.000000000000000000 ) ) ;
#1828 = ORIENTED_EDGE ( 'NONE', *, *, #9081, .T. ) ;
#1829 = CIRCLE ( 'NONE', #11373, 0.7849999999999983658 ) ;
#1830 = CARTESIAN_POINT ( 'NONE',  ( 0.7238772453881168190, -0.4379537528022394710, 0.4547576871318959602 ) ) ;
#1831 = DIRECTION ( 'NONE',  ( 0.000000000000000000, 1.000000000000000000, 0.000000000000000000 ) ) ;
#1832 = ORIENTED_EDGE ( 'NONE', *, *, #13509, .T. ) ;
#1833 = CIRCLE ( 'NONE', #13796, 1.039370078740158965 ) ;
#1834 = CIRCLE ( 'NONE', #9434, 0.2625000000000000111 ) ;
#1835 = EDGE_CURVE ( 'NONE', #3706, #11962, #3308, .T. ) ;
#1836 = CARTESIAN_POINT ( 'NONE',  ( 0.6179999999999965521, 1.679378605318035733, -1.679378605318065487 ) ) ;
#1837 = ORIENTED_EDGE ( 'NONE', *, *, #10304, .T. ) ;
#1838 =( NAMED_UNIT ( * ) PLANE_ANGLE_UNIT ( ) SI_UNIT ( $, .RADIAN. ) );
#1839 = CARTESIAN_POINT ( 'NONE',  ( -0.4424999999999983946, -0.6590000000000000302, -0.3725000000000000533 ) ) ;
#1840 = AXIS2_PLACEMENT_3D ( 'NONE', #1985, #1365, #12767 ) ;
#1841 = FILL_AREA_STYLE ('',( #8472 ) ) ;
#1842 = CARTESIAN_POINT ( 'NONE',  ( 0.8296723582540662667, -0.4310852393111275216, -0.3487905724596098711 ) ) ;
#1843 = CARTESIAN_POINT ( 'NONE',  ( 0.9669439593609970851, -0.4433899119250455101, -0.4088229889177615872 ) ) ;
#1844 = VECTOR ( 'NONE', #14742, 39.37007874015748143 ) ;
#1845 = CIRCLE ( 'NONE', #9687, 1.000000000000000222 ) ;
#1846 = ORIENTED_EDGE ( 'NONE', *, *, #10065, .F. ) ;
#1847 = CARTESIAN_POINT ( 'NONE',  ( 3.426491571325181340, -3.360000000000016751, -0.9799999999999434719 ) ) ;
#1848 = CARTESIAN_POINT ( 'NONE',  ( -0.4424999999999985056, -0.6590000000000000302, -0.8499999999999999778 ) ) ;
#1849 = APPLICATION_CONTEXT ( 'automotive_design' ) ;
#1850 = CARTESIAN_POINT ( 'NONE',  ( 3.426491571325181340, -2.359999999999984333, 1.575000000000016387 ) ) ;
#1851 = ORIENTED_EDGE ( 'NONE', *, *, #10999, .F. ) ;
#1852 = ORIENTED_EDGE ( 'NONE', *, *, #4932, .T. ) ;
#1853 = VECTOR ( 'NONE', #12516, 39.37007874015748143 ) ;
#1854 = ORIENTED_EDGE ( 'NONE', *, *, #9770, .T. ) ;
#1855 = CARTESIAN_POINT ( 'NONE',  ( 3.944129661530210385, 2.366055667732568841E-16, -1.932031071636253650 ) ) ;
#1856 = EDGE_CURVE ( 'NONE', #11895, #11673, #10715, .T. ) ;
#1857 = CARTESIAN_POINT ( 'NONE',  ( 2.774999999999999911, 2.399999999999999911, -0.7000000000000009548 ) ) ;
#1858 = CARTESIAN_POINT ( 'NONE',  ( 3.875000000000000000, 3.535499999999999865, 0.000000000000000000 ) ) ;
#1859 = ADVANCED_FACE ( 'NONE', ( #3231 ), #6825, .T. ) ;
#1860 = DIRECTION ( 'NONE',  ( 0.000000000000000000, 0.000000000000000000, -1.000000000000000000 ) ) ;
#1861 = CIRCLE ( 'NONE', #4570, 0.2624999999999994560 ) ;
#1862 = ORIENTED_EDGE ( 'NONE', *, *, #529, .F. ) ;
#1863 = VECTOR ( 'NONE', #12907, 39.37007874015748854 ) ;
#1864 = ORIENTED_EDGE ( 'NONE', *, *, #8532, .T. ) ;
#1865 = VERTEX_POINT ( 'NONE', #7896 ) ;
#1866 = VERTEX_POINT ( 'NONE', #6759 ) ;
#1867 = DIRECTION ( 'NONE',  ( 0.000000000000000000, 0.000000000000000000, 1.000000000000000000 ) ) ;
#1868 = CARTESIAN_POINT ( 'NONE',  ( 3.875000000000000000, 1.885381157978845312, 0.5000000000000002220 ) ) ;
#1869 = DIRECTION ( 'NONE',  ( 1.000000000000000000, 0.000000000000000000, 0.000000000000000000 ) ) ;
#1870 = CONICAL_SURFACE ( 'NONE', #7037, 0.2041999999999996596, 0.7853981633974460586 ) ;
#1871 = CONTEXT_DEPENDENT_SHAPE_REPRESENTATION ( #2304, #10084 ) ;
#1872 = DIRECTION ( 'NONE',  ( -0.000000000000000000, -1.000000000000000000, 0.000000000000000000 ) ) ;
#1873 = ORIENTED_EDGE ( 'NONE', *, *, #3850, .T. ) ;
#1874 = CARTESIAN_POINT ( 'NONE',  ( 3.875000000000000000, 3.137999999999999901, -0.5000000000000002220 ) ) ;
#1875 = CARTESIAN_POINT ( 'NONE',  ( 0.8999999999999999112, -0.6429999999999999050, -0.3750000000000000555 ) ) ;
#1876 = EDGE_CURVE ( 'NONE', #4934, #13039, #9514, .T. ) ;
#1877 = ADVANCED_FACE ( 'NONE', ( #4309 ), #8035, .F. ) ;
#1878 = CARTESIAN_POINT ( 'NONE',  ( 0.6179999999999962190, -1.679378605318048390, 2.054378605318054607 ) ) ;
#1879 = DIRECTION ( 'NONE',  ( -0.000000000000000000, -1.000000000000000000, -0.000000000000000000 ) ) ;
#1880 = CIRCLE ( 'NONE', #4091, 0.7849999999999998090 ) ;
#1881 = CARTESIAN_POINT ( 'NONE',  ( 2.774999999999999911, -2.360000000000021636, -1.574999999999999734 ) ) ;
#1882 = CARTESIAN_POINT ( 'NONE',  ( 2.774999999999999911, 1.679378605318059048, 1.384878605318040856 ) ) ;
#1883 = CARTESIAN_POINT ( 'NONE',  ( 4.505898589230239004, 1.711421573918742833, 0.4949957780824733589 ) ) ;
#1885 = ORIENTED_EDGE ( 'NONE', *, *, #5208, .T. ) ;
#1884 = CARTESIAN_POINT ( 'NONE',  ( 3.851496678973868271, 1.891896550263048038, -0.5000000000000002220 ) ) ;
#1886 = CIRCLE ( 'NONE', #12890, 0.4070000000000058016 ) ;
#1887 = EDGE_LOOP ( 'NONE', ( #3497, #11766, #4798, #3666 ) ) ;
#1889 = ORIENTED_EDGE ( 'NONE', *, *, #8087, .T. ) ;
#1888 = DIRECTION ( 'NONE',  ( 0.000000000000000000, 0.000000000000000000, -1.000000000000000000 ) ) ;
#1890 = ORIENTED_EDGE ( 'NONE', *, *, #1373, .F. ) ;
#1891 = AXIS2_PLACEMENT_3D ( 'NONE', #2753, #4049, #8717 ) ;
#1892 = DIRECTION ( 'NONE',  ( 0.7071067811865460184, 0.000000000000000000, -0.7071067811865490160 ) ) ;
#1893 = DIRECTION ( 'NONE',  ( 0.000000000000000000, 0.000000000000000000, -1.000000000000000000 ) ) ;
#1894 = ORIENTED_EDGE ( 'NONE', *, *, #4747, .F. ) ;
#1895 = LINE ( 'NONE', #511, #3804 ) ;
#1896 = FACE_OUTER_BOUND ( 'NONE', #298, .T. ) ;
#1897 = AXIS2_PLACEMENT_3D ( 'NONE', #2646, #7325, #8613 ) ;
#1898 = AXIS2_PLACEMENT_3D ( 'NONE', #9262, #971, #7875 ) ;
#1899 = CARTESIAN_POINT ( 'NONE',  ( 0.1807106342563528367, 1.629999999999999893, 5.178337979384803075E-18 ) ) ;
#1900 = CARTESIAN_POINT ( 'NONE',  ( 2.774999999999999911, -1.679378605318041950, 1.679378605318059048 ) ) ;
#1901 = ORIENTED_EDGE ( 'NONE', *, *, #5473, .T. ) ;
#1902 = CARTESIAN_POINT ( 'NONE',  ( 3.085497600961857767, 0.7407061222255643118, 0.4564195254101433008 ) ) ;
#1903 = VECTOR ( 'NONE', #3768, 39.37007874015748143 ) ;
#1904 = CARTESIAN_POINT ( 'NONE',  ( 3.381634859058371578, 0.9966950651981517639, 0.08284753930692498325 ) ) ;
#1905 = VECTOR ( 'NONE', #3519, 39.37007874015748854 ) ;
#1906 = CARTESIAN_POINT ( 'NONE',  ( 4.393322081076587615, 1.706995504219652737, -0.6070895335983141905 ) ) ;
#1907 = VERTEX_POINT ( 'NONE', #9054 ) ;
#1908 = CIRCLE ( 'NONE', #6327, 0.1000000000000000194 ) ;
#1909 = CARTESIAN_POINT ( 'NONE',  ( 0.09500000000000431710, -1.679378605318047946, -1.679378605318053497 ) ) ;
#1910 = LINE ( 'NONE', #3296, #3577 ) ;
#1911 = ORIENTED_EDGE ( 'NONE', *, *, #6818, .F. ) ;
#1912 = CONICAL_SURFACE ( 'NONE', #439, 0.3750000000000004996, 0.7853981633974547183 ) ;
#1913 = DIRECTION ( 'NONE',  ( -1.000000000000000000, -0.000000000000000000, -0.000000000000000000 ) ) ;
#1914 = EDGE_LOOP ( 'NONE', ( #9355, #9384, #9462, #9325 ) ) ;
#1915 = ADVANCED_FACE ( 'NONE', ( #1991 ), #14708, .T. ) ;
#1916 =( LENGTH_UNIT ( ) NAMED_UNIT ( * ) SI_UNIT ( $, .METRE. ) );
#1917 = CARTESIAN_POINT ( 'NONE',  ( 0.9749999999999999778, -0.4829448521957645513, -0.3750000000000000555 ) ) ;
#1918 = EDGE_CURVE ( 'NONE', #6363, #10392, #1171, .T. ) ;
#1919 = AXIS2_PLACEMENT_3D ( 'NONE', #12528, #11247, #742 ) ;
#1920 = CARTESIAN_POINT ( 'NONE',  ( 3.426491571325181340, 2.062169880637645836, -0.5999481385559802815 ) ) ;
#1921 = CARTESIAN_POINT ( 'NONE',  ( 1.860560713453747184, -0.1867359432429938626, 0.4737208938777718870 ) ) ;
#1922 =( LENGTH_UNIT ( ) NAMED_UNIT ( * ) SI_UNIT ( $, .METRE. ) );
#1923 = DIRECTION ( 'NONE',  ( -0.000000000000000000, 1.000000000000000000, -0.000000000000000000 ) ) ;
#1924 = TOROIDAL_SURFACE ( 'NONE', #10492, 0.7057575716915831521, 0.04000000000000000083 ) ;
#1925 = DIRECTION ( 'NONE',  ( 0.7071067811865336949, 0.7071067811865612285, 0.000000000000000000 ) ) ;
#1926 = AXIS2_PLACEMENT_3D ( 'NONE', #3018, #9907, #14483 ) ;
#1927 = ORIENTED_EDGE ( 'NONE', *, *, #10850, .F. ) ;
#1928 = ADVANCED_FACE ( 'NONE', ( #7668, #5532 ), #1764, .T. ) ;
#1929 = DIRECTION ( 'NONE',  ( -1.000000000000000000, -0.000000000000000000, -0.000000000000000000 ) ) ;
#1930 = CARTESIAN_POINT ( 'NONE',  ( 2.775039370078740131, 1.679378605318059492, 1.679378605318041506 ) ) ;
#1931 = CARTESIAN_POINT ( 'NONE',  ( 0.7023826192914042199, -0.3918571065744204107, -0.4896101277505874316 ) ) ;
#1932 = ORIENTED_EDGE ( 'NONE', *, *, #977, .F. ) ;
#1933 = ORIENTED_EDGE ( 'NONE', *, *, #973, .T. ) ;
#1934 = DIRECTION ( 'NONE',  ( -0.4919537527695821422, 0.04988190024277998347, -0.8691911764186832645 ) ) ;
#1935 = VERTEX_POINT ( 'NONE', #2069 ) ;
#1936 = CIRCLE ( 'NONE', #4635, 0.4850000000000000977 ) ;
#1937 = DIRECTION ( 'NONE',  ( 0.000000000000000000, 0.000000000000000000, -1.000000000000000000 ) ) ;
#1938 = EDGE_CURVE ( 'NONE', #12744, #6280, #194, .T. ) ;
#1939 = DIRECTION ( 'NONE',  ( -0.000000000000000000, -1.000000000000000000, -0.000000000000000000 ) ) ;
#1940 = AXIS2_PLACEMENT_3D ( 'NONE', #8894, #6523, #8976 ) ;
#1941 = ADVANCED_FACE ( 'NONE', ( #8825 ), #9513, .F. ) ;
#1942 = CARTESIAN_POINT ( 'NONE',  ( 3.875000000000000000, 3.170499999999999208, 0.4849999999999995981 ) ) ;
#1943 = DIRECTION ( 'NONE',  ( -1.000000000000000000, -0.000000000000000000, -0.000000000000000000 ) ) ;
#1944 = ORIENTED_EDGE ( 'NONE', *, *, #7030, .T. ) ;
#1945 = ADVANCED_FACE ( 'NONE', ( #1299 ), #15006, .T. ) ;
#1946 = CIRCLE ( 'NONE', #9301, 2.500000000000000000 ) ;
#1947 = CARTESIAN_POINT ( 'NONE',  ( 4.051235613900670884, 1.808866337081830311, -0.7302300179307213979 ) ) ;
#1948 = EDGE_LOOP ( 'NONE', ( #4251, #8463, #4769, #134 ) ) ;
#1949 = EDGE_LOOP ( 'NONE', ( #8429, #14296, #3758, #2440 ) ) ;
#1950 = EDGE_CURVE ( 'NONE', #13688, #8873, #4111, .T. ) ;
#1951 = ORIENTED_EDGE ( 'NONE', *, *, #12872, .F. ) ;
#1952 = CARTESIAN_POINT ( 'NONE',  ( 3.897980617091954869, 1.879010665267595304, -0.5000000000000002220 ) ) ;
#1953 = DIRECTION ( 'NONE',  ( 0.000000000000000000, 0.000000000000000000, -1.000000000000000000 ) ) ;
#1954 = DIRECTION ( 'NONE',  ( 0.000000000000000000, 0.000000000000000000, -1.000000000000000000 ) ) ;
#1955 = DIRECTION ( 'NONE',  ( -0.8682164115033652596, 8.537024980200830693E-16, -0.4961857140186719528 ) ) ;
#1956 = ORIENTED_EDGE ( 'NONE', *, *, #2136, .F. ) ;
#1957 = LINE ( 'NONE', #2102, #8319 ) ;
#1958 = DIRECTION ( 'NONE',  ( -0.8682164115033652596, 0.000000000000000000, -0.4961857140186719528 ) ) ;
#1959 = EDGE_CURVE ( 'NONE', #2642, #12259, #3535, .T. ) ;
#1960 = DIRECTION ( 'NONE',  ( 0.000000000000000000, 0.000000000000000000, -1.000000000000000000 ) ) ;
#1961 = AXIS2_PLACEMENT_3D ( 'NONE', #9620, #11183, #6247 ) ;
#1962 = CARTESIAN_POINT ( 'NONE',  ( 4.541376298268983369, 1.714299675483434982, 0.4487873714220094734 ) ) ;
#1964 = ORIENTED_EDGE ( 'NONE', *, *, #13004, .T. ) ;
#1963 = CARTESIAN_POINT ( 'NONE',  ( 0.000000000000000000, 0.000000000000000000, 0.000000000000000000 ) ) ;
#1965 = EDGE_CURVE ( 'NONE', #11671, #14534, #12647, .T. ) ;
#1966 = ORIENTED_EDGE ( 'NONE', *, *, #2823, .F. ) ;
#1968 = ORIENTED_EDGE ( 'NONE', *, *, #529, .T. ) ;
#1967 = DIRECTION ( 'NONE',  ( 0.7071067811865464625, -0.7071067811865486830, 0.000000000000000000 ) ) ;
#1969 = VERTEX_POINT ( 'NONE', #5987 ) ;
#1970 = DIRECTION ( 'NONE',  ( -1.000000000000000000, -0.000000000000000000, -0.000000000000000000 ) ) ;
#1971 = CARTESIAN_POINT ( 'NONE',  ( 0.1250000000000009992, 1.224646799147353207E-16, -1.000000000000000000 ) ) ;
#1972 = VERTEX_POINT ( 'NONE', #10652 ) ;
#1973 = DIRECTION ( 'NONE',  ( 0.000000000000000000, 0.000000000000000000, -1.000000000000000000 ) ) ;
#1974 = DIRECTION ( 'NONE',  ( -0.000000000000000000, 1.000000000000000000, -0.000000000000000000 ) ) ;
#1975 = AXIS2_PLACEMENT_3D ( 'NONE', #6108, #9693, #14267 ) ;
#1976 = CARTESIAN_POINT ( 'NONE',  ( 2.599715518929682556, 0.7930078835992490083, -0.4632808542524021744 ) ) ;
#1977 = CARTESIAN_POINT ( 'NONE',  ( 0.9719599677838458573, -0.4431686115285130012, -0.3970034835699213782 ) ) ;
#1978 = EDGE_LOOP ( 'NONE', ( #12904, #37, #2076, #7563 ) ) ;
#1979 = DIRECTION ( 'NONE',  ( -0.01412288512831213171, 3.675428035873182550E-19, -0.9999002670844991947 ) ) ;
#1980 = CARTESIAN_POINT ( 'NONE',  ( 3.510247954615316246, 0.9396455958913839668, -0.3423636469962711981 ) ) ;
#1981 = DIRECTION ( 'NONE',  ( -1.000000000000000000, 0.000000000000000000, 0.000000000000000000 ) ) ;
#1982 = EDGE_CURVE ( 'NONE', #5653, #11004, #3149, .T. ) ;
#1983 = COLOUR_RGB ( '',0.7921568627450980005, 0.8196078431372548767, 0.9333333333333333481 ) ;
#1984 = LINE ( 'NONE', #14619, #13797 ) ;
#1985 = CARTESIAN_POINT ( 'NONE',  ( 3.874999999999999556, 3.535499999999999421, 1.320000000000000062 ) ) ;
#1986 = VERTEX_POINT ( 'NONE', #5686 ) ;
#1987 = CARTESIAN_POINT ( 'NONE',  ( -0.3724999999999999423, 0.000000000000000000, -0.4124999999999999778 ) ) ;
#1988 = ORIENTED_EDGE ( 'NONE', *, *, #2996, .T. ) ;
#1989 = CARTESIAN_POINT ( 'NONE',  ( 0.7134904538003048469, -0.4429999999999998939, -0.4077598229816901121 ) ) ;
#1990 = CARTESIAN_POINT ( 'NONE',  ( 3.874999999999999556, 3.535499999999999421, 1.320000000000000062 ) ) ;
#1991 = FACE_OUTER_BOUND ( 'NONE', #2900, .T. ) ;
#1992 = VERTEX_POINT ( 'NONE', #6989 ) ;
#1993 = DIRECTION ( 'NONE',  ( -0.7070715176384873013, -0.7070715176384764211, 0.009986885842350509690 ) ) ;
#1994 = DIRECTION ( 'NONE',  ( 0.000000000000000000, 0.000000000000000000, 1.000000000000000000 ) ) ;
#1995 = LINE ( 'NONE', #5621, #7963 ) ;
#1996 = ORIENTED_EDGE ( 'NONE', *, *, #8488, .T. ) ;
#1997 = VERTEX_POINT ( 'NONE', #11497 ) ;
#1998 = VECTOR ( 'NONE', #2700, 39.37007874015748143 ) ;
#1999 = DIRECTION ( 'NONE',  ( -0.000000000000000000, -1.000000000000000000, -0.000000000000000000 ) ) ;
#2000 = ORIENTED_EDGE ( 'NONE', *, *, #12278, .F. ) ;
#2001 = CARTESIAN_POINT ( 'NONE',  ( 2.814370078740158210, 0.000000000000000000, 1.000000000000000000 ) ) ;
#2002 = DIRECTION ( 'NONE',  ( 0.9396926207859108704, -0.000000000000000000, 0.3420201433256621626 ) ) ;
#2003 = CARTESIAN_POINT ( 'NONE',  ( 2.774999999999999911, -1.679378605318059048, -1.973878605318027724 ) ) ;
#2004 = AXIS2_PLACEMENT_3D ( 'NONE', #13432, #5345, #14671 ) ;
#2005 = CARTESIAN_POINT ( 'NONE',  ( 0.000000000000000000, 1.249999999999999778, 0.000000000000000000 ) ) ;
#2006 = CIRCLE ( 'NONE', #8148, 0.2944999999999987073 ) ;
#2007 = DIRECTION ( 'NONE',  ( 0.000000000000000000, 0.000000000000000000, -1.000000000000000000 ) ) ;
#2008 = VERTEX_POINT ( 'NONE', #9437 ) ;
#2009 = DIRECTION ( 'NONE',  ( -1.000000000000000000, -0.000000000000000000, -0.000000000000000000 ) ) ;
#2010 = EDGE_CURVE ( 'NONE', #3074, #2140, #14370, .T. ) ;
#2011 = ADVANCED_FACE ( 'NONE', ( #15084 ), #12857, .F. ) ;
#2012 = EDGE_CURVE ( 'NONE', #6058, #13458, #8301, .T. ) ;
#2013 = CONICAL_SURFACE ( 'NONE', #1540, 0.2625000000000000111, 0.7853981633974452814 ) ;
#2014 = CARTESIAN_POINT ( 'NONE',  ( 4.119080202121599754, 1.796483476452471972, -0.7105853202116764189 ) ) ;
#2015 = ORIENTED_EDGE ( 'NONE', *, *, #14265, .F. ) ;
#2016 = VERTEX_POINT ( 'NONE', #145 ) ;
#2017 = ORIENTED_EDGE ( 'NONE', *, *, #12262, .F. ) ;
#2018 = CARTESIAN_POINT ( 'NONE',  ( 3.600570009308222907, 1.057000000000000162, -0.3891385068221628885 ) ) ;
#2019 = CYLINDRICAL_SURFACE ( 'NONE', #1614, 0.9499999999999988454 ) ;
#2020 = PLANE ( 'NONE',  #686 ) ;
#2021 = EDGE_CURVE ( 'NONE', #4636, #8991, #5843, .T. ) ;
#2022 = CARTESIAN_POINT ( 'NONE',  ( -0.2099999999999948852, 1.559103846021543616, 0.3809527529760087239 ) ) ;
#2023 = EDGE_LOOP ( 'NONE', ( #13714, #5234, #13749, #918 ) ) ;
#2024 = CARTESIAN_POINT ( 'NONE',  ( 3.162550611401342415, 2.489436539607832621, 0.2300036551928836270 ) ) ;
#2025 = CARTESIAN_POINT ( 'NONE',  ( 0.6566433263006997700, -0.01168724275744807174, -0.4973513887421225910 ) ) ;
#2026 = CIRCLE ( 'NONE', #3767, 0.5175000000000000711 ) ;
#2027 = VECTOR ( 'NONE', #1063, 39.37007874015748143 ) ;
#2028 = FACE_OUTER_BOUND ( 'NONE', #12492, .T. ) ;
#2029 = CARTESIAN_POINT ( 'NONE',  ( 0.8819080671433473517, -0.4426951315057036096, -0.4482526998616632730 ) ) ;
#2030 = CARTESIAN_POINT ( 'NONE',  ( 4.150492928931191372, 1.791887721204809214, 0.6990997386737194397 ) ) ;
#2032 = ORIENTED_EDGE ( 'NONE', *, *, #3818, .T. ) ;
#2031 = CARTESIAN_POINT ( 'NONE',  ( 3.405153689607044232, 3.137999999999999901, 1.491010071662831171 ) ) ;
#2033 = EDGE_LOOP ( 'NONE', ( #14997, #9064, #3093, #729 ) ) ;
#2034 = AXIS2_PLACEMENT_3D ( 'NONE', #14943, #3141, #813 ) ;
#2036 = VERTEX_POINT ( 'NONE', #12628 ) ;
#2035 = CYLINDRICAL_SURFACE ( 'NONE', #14080, 0.05999999999999992839 ) ;
#2037 = ORIENTED_EDGE ( 'NONE', *, *, #11368, .F. ) ;
#2038 = CYLINDRICAL_SURFACE ( 'NONE', #3134, 0.06000000000000001166 ) ;
#2039 = CARTESIAN_POINT ( 'NONE',  ( 3.874999999999999556, 3.137999999999999901, 1.320000000000000062 ) ) ;
#2040 = EDGE_LOOP ( 'NONE', ( #10640, #4681, #5070, #5535 ) ) ;
#2041 = DIRECTION ( 'NONE',  ( 0.000000000000000000, 0.000000000000000000, 1.000000000000000000 ) ) ;
#2042 = DIRECTION ( 'NONE',  ( -1.000000000000000000, -0.000000000000000000, -0.000000000000000000 ) ) ;
#2043 = EDGE_CURVE ( 'NONE', #1986, #6203, #5310, .T. ) ;
#2044 = FACE_OUTER_BOUND ( 'NONE', #14825, .T. ) ;
#2045 = EDGE_CURVE ( 'NONE', #13550, #10543, #10504, .T. ) ;
#2046 = CARTESIAN_POINT ( 'NONE',  ( 2.187203820042823654, 0.4712135623730920875, -0.4085020630706684974 ) ) ;
#2047 = CIRCLE ( 'NONE', #10617, 1.000000000000000222 ) ;
#2048 = CARTESIAN_POINT ( 'NONE',  ( 0.9745723538550742360, -0.4432286986229772574, -0.3850634666812919882 ) ) ;
#2049 = AXIS2_PLACEMENT_3D ( 'NONE', #7498, #7477, #6036 ) ;
#2050 = ORIENTED_EDGE ( 'NONE', *, *, #3630, .T. ) ;
#2051 = CYLINDRICAL_SURFACE ( 'NONE', #9263, 0.2624999999999997335 ) ;
#2052 = CARTESIAN_POINT ( 'NONE',  ( 3.852151642586534308, 1.889461949475109925, 0.5000000000000286438 ) ) ;
#2053 = DIRECTION ( 'NONE',  ( 0.000000000000000000, 0.000000000000000000, -1.000000000000000000 ) ) ;
#2054 = CARTESIAN_POINT ( 'NONE',  ( 2.774999999999999911, 2.360000000000015863, 1.574999999999999956 ) ) ;
#2056 = ORIENTED_EDGE ( 'NONE', *, *, #1007, .T. ) ;
#2055 = DIRECTION ( 'NONE',  ( 0.000000000000000000, 0.7071067811865509034, 0.7071067811865441310 ) ) ;
#2057 = VERTEX_POINT ( 'NONE', #1228 ) ;
#2058 = DIRECTION ( 'NONE',  ( -1.000000000000000000, -1.837151692781460616E-16, 0.000000000000000000 ) ) ;
#2059 = ORIENTED_EDGE ( 'NONE', *, *, #2359, .T. ) ;
#2060 = CARTESIAN_POINT ( 'NONE',  ( 3.426491571325181340, 1.954234464180151676, 0.6847610993685215863 ) ) ;
#2061 = CIRCLE ( 'NONE', #13783, 1.000000000000000222 ) ;
#2062 = CIRCLE ( 'NONE', #8198, 0.05999999999999997696 ) ;
#2063 =( BOUNDED_CURVE ( )  B_SPLINE_CURVE ( 3, ( #7705, #5648, #13729, #11372 ),
 .UNSPECIFIED., .F., .T. ) 
 B_SPLINE_CURVE_WITH_KNOTS ( ( 4, 4 ),
 ( 4.726512335037234891, 6.283185307179586232 ),
 .UNSPECIFIED. ) 
 CURVE ( )  GEOMETRIC_REPRESENTATION_ITEM ( )  RATIONAL_B_SPLINE_CURVE ( ( 1.000000000000000000, 0.8080549792898082950, 0.8080549792898082950, 1.000000000000000000 ) ) 
 REPRESENTATION_ITEM ( '' )  );
#2064 = EDGE_CURVE ( 'NONE', #9791, #4426, #11702, .T. ) ;
#2065 = EDGE_CURVE ( 'NONE', #1001, #8481, #15102, .T. ) ;
#2066 = CARTESIAN_POINT ( 'NONE',  ( 1.886302412727927758, -0.2406659208688838592, 0.4137268778526354551 ) ) ;
#2067 = CARTESIAN_POINT ( 'NONE',  ( 0.6940843099860020127, -0.4844395605446530917, -0.4145488311989724561 ) ) ;
#2068 = DIRECTION ( 'NONE',  ( 0.000000000000000000, 0.000000000000000000, 1.000000000000000000 ) ) ;
#2069 = CARTESIAN_POINT ( 'NONE',  ( 2.743000000000000771, 1.679378605318059048, 1.941878605318041240 ) ) ;
#2070 = ORIENTED_EDGE ( 'NONE', *, *, #4974, .T. ) ;
#2071 = CIRCLE ( 'NONE', #6980, 0.2624999999999997335 ) ;
#2072 = DIRECTION ( 'NONE',  ( 0.000000000000000000, 1.000000000000000000, 0.000000000000000000 ) ) ;
#2073 = DIRECTION ( 'NONE',  ( 0.000000000000000000, 1.000000000000000000, 0.000000000000000000 ) ) ;
#2074 = AXIS2_PLACEMENT_3D ( 'NONE', #14602, #5434, #2982 ) ;
#2075 = CARTESIAN_POINT ( 'NONE',  ( -0.4125000000000001998, 0.1859999999999983611, -0.3725000000000000533 ) ) ;
#2076 = ORIENTED_EDGE ( 'NONE', *, *, #9463, .F. ) ;
#2077 = CARTESIAN_POINT ( 'NONE',  ( 0.6500000000000001332, -1.679378605318047946, -1.679378605318053497 ) ) ;
#2078 = CARTESIAN_POINT ( 'NONE',  ( 3.874999999999999556, 3.137999999999999901, -1.542500000000001315 ) ) ;
#2079 = DIRECTION ( 'NONE',  ( 0.000000000000000000, 0.000000000000000000, 1.000000000000000000 ) ) ;
#2080 = VERTEX_POINT ( 'NONE', #6841 ) ;
#2081 = CARTESIAN_POINT ( 'NONE',  ( 2.980731298636167370, 3.137999999999999901, -0.3249191361593797844 ) ) ;
#2082 = CARTESIAN_POINT ( 'NONE',  ( 0.6678750254534769892, -0.4638942219540296286, -0.4666347774677366278 ) ) ;
#2083 = CONICAL_SURFACE ( 'NONE', #14299, 0.4070000000000025264, 0.7853981633974557175 ) ;
#2084 = CARTESIAN_POINT ( 'NONE',  ( 0.6179999999999965521, 1.679378605318035733, -1.679378605318065487 ) ) ;
#2085 = CONICAL_SURFACE ( 'NONE', #4310, 0.2812500000000000555, 0.7853981633974465026 ) ;
#2086 = AXIS2_PLACEMENT_3D ( 'NONE', #1730, #6700, #1018 ) ;
#2087 = CARTESIAN_POINT ( 'NONE',  ( 3.449073513670800839, 2.047967394769590666, 0.2629493547202494952 ) ) ;
#2088 = EDGE_CURVE ( 'NONE', #8835, #7795, #11570, .T. ) ;
#2089 = ORIENTED_EDGE ( 'NONE', *, *, #7219, .T. ) ;
#2090 = CIRCLE ( 'NONE', #13562, 0.05999999999999990757 ) ;
#2091 = SHAPE_REPRESENTATION ( 'Ball Valve Sub', ( #8424 ), #10122 ) ;
#2092 = ORIENTED_EDGE ( 'NONE', *, *, #4474, .T. ) ;
#2093 = VERTEX_POINT ( 'NONE', #70 ) ;
#2094 = CIRCLE ( 'NONE', #4312, 0.1899999999999996136 ) ;
#2095 = LINE ( 'NONE', #10370, #12837 ) ;
#2096 = EDGE_LOOP ( 'NONE', ( #8056, #11237, #5998, #11561 ) ) ;
#2097 = DIRECTION ( 'NONE',  ( 0.000000000000000000, 0.000000000000000000, -1.000000000000000000 ) ) ;
#2098 = DIRECTION ( 'NONE',  ( 1.000000000000000000, 0.000000000000000000, 0.000000000000000000 ) ) ;
#2099 = LINE ( 'NONE', #6786, #13646 ) ;
#2100 = CARTESIAN_POINT ( 'NONE',  ( -0.01818920831125185600, 1.603403463250997474, 0.3809527529760087239 ) ) ;
#2101 = VERTEX_POINT ( 'NONE', #4764 ) ;
#2102 = CARTESIAN_POINT ( 'NONE',  ( 6.826491571325181695, 1.679378605318059492, 1.304378605318041062 ) ) ;
#2103 = EDGE_CURVE ( 'NONE', #4450, #7612, #7070, .T. ) ;
#2104 = EDGE_CURVE ( 'NONE', #4855, #12193, #5103, .T. ) ;
#2105 = VECTOR ( 'NONE', #3669, 39.37007874015748143 ) ;
#2106 = CARTESIAN_POINT ( 'NONE',  ( 0.7350000851713978101, -0.001253058305733974198, -0.4439478790714003753 ) ) ;
#2107 = EDGE_CURVE ( 'NONE', #10756, #5850, #3697, .T. ) ;
#2108 = CARTESIAN_POINT ( 'NONE',  ( 3.874999999999999556, 3.567999999999999616, -1.820000000000000284 ) ) ;
#2109 = DIRECTION ( 'NONE',  ( 0.000000000000000000, 0.000000000000000000, 1.000000000000000000 ) ) ;
#2110 = EDGE_CURVE ( 'NONE', #11380, #1972, #10233, .T. ) ;
#2111 = CARTESIAN_POINT ( 'NONE',  ( 4.601389648059055482, 1.745381240488223629, 0.1935210130979204968 ) ) ;
#2113 = EDGE_LOOP ( 'NONE', ( #10769, #4278, #3503, #5803 ) ) ;
#2112 = CARTESIAN_POINT ( 'NONE',  ( 6.826491571325181695, 0.000000000000000000, 0.000000000000000000 ) ) ;
#2114 = CIRCLE ( 'NONE', #9214, 0.07000000000000047851 ) ;
#2115 = ORIENTED_EDGE ( 'NONE', *, *, #12591, .F. ) ;
#2117 = ORIENTED_EDGE ( 'NONE', *, *, #5961, .T. ) ;
#2116 = CARTESIAN_POINT ( 'NONE',  ( 3.426491571325181340, 0.000000000000000000, 0.000000000000000000 ) ) ;
#2118 = ORIENTED_EDGE ( 'NONE', *, *, #14501, .T. ) ;
#2119 = FACE_BOUND ( 'NONE', #5327, .T. ) ;
#2120 = CARTESIAN_POINT ( 'NONE',  ( 3.234999999999998543, -1.679378605318041728, 1.679378605318059048 ) ) ;
#2121 = DIRECTION ( 'NONE',  ( 1.000000000000000000, 0.000000000000000000, 0.000000000000000000 ) ) ;
#2122 = EDGE_LOOP ( 'NONE', ( #899, #5832, #13565, #8919 ) ) ;
#2123 = DIRECTION ( 'NONE',  ( -0.000000000000000000, -1.000000000000000000, -0.000000000000000000 ) ) ;
#2124 = CARTESIAN_POINT ( 'NONE',  ( 0.6866196799637447334, -0.4820297792901954703, -0.4282732318476363265 ) ) ;
#2125 = EDGE_CURVE ( 'NONE', #6934, #2859, #6142, .T. ) ;
#2126 = CONICAL_SURFACE ( 'NONE', #8001, 0.2945000000000009277, 0.7853981633974503884 ) ;
#2127 = DIRECTION ( 'NONE',  ( 0.9999002670844991947, 1.365787769249574922E-16, 0.01412288512831213171 ) ) ;
#2128 = FACE_OUTER_BOUND ( 'NONE', #2113, .T. ) ;
#2129 = CARTESIAN_POINT ( 'NONE',  ( 0.6179999999999965521, 1.679378605318035733, -1.304378605318064821 ) ) ;
#2130 = CYLINDRICAL_SURFACE ( 'NONE', #3086, 2.500000000000000000 ) ;
#2131 = CIRCLE ( 'NONE', #2426, 0.05999999999999994227 ) ;
#2132 = DIRECTION ( 'NONE',  ( -1.000000000000000000, -0.000000000000000000, -0.000000000000000000 ) ) ;
#2133 = CARTESIAN_POINT ( 'NONE',  ( 3.712234661458500007, 0.8810498532991303255, -0.4730558837152146201 ) ) ;
#2134 = CIRCLE ( 'NONE', #2641, 0.06000000000000004635 ) ;
#2135 = CARTESIAN_POINT ( 'NONE',  ( 3.968383684466501915, 1.755580462719493973, -0.7909561288026154546 ) ) ;
#2136 = EDGE_CURVE ( 'NONE', #6629, #11132, #6367, .T. ) ;
#2137 = DIRECTION ( 'NONE',  ( 0.000000000000000000, 0.000000000000000000, -1.000000000000000000 ) ) ;
#2139 = ORIENTED_EDGE ( 'NONE', *, *, #4405, .F. ) ;
#2138 = DIRECTION ( 'NONE',  ( 0.7071067811865466846, -0.7071067811865483499, 0.000000000000000000 ) ) ;
#2140 = VERTEX_POINT ( 'NONE', #6063 ) ;
#2141 = EDGE_CURVE ( 'NONE', #8364, #1193, #9801, .T. ) ;
#2142 = DIRECTION ( 'NONE',  ( 0.000000000000000000, 0.000000000000000000, -1.000000000000000000 ) ) ;
#2143 = EDGE_LOOP ( 'NONE', ( #7259, #9599, #13875, #13158 ) ) ;
#2144 = DIRECTION ( 'NONE',  ( 0.000000000000000000, 1.000000000000000000, 0.000000000000000000 ) ) ;
#2145 = VECTOR ( 'NONE', #5684, 39.37007874015748143 ) ;
#2146 = CARTESIAN_POINT ( 'NONE',  ( 3.241046123363275022, 0.7391609583210635437, -0.4542225123818747212 ) ) ;
#2147 = DIRECTION ( 'NONE',  ( -1.000000000000000000, -0.000000000000000000, -0.000000000000000000 ) ) ;
#2148 = CYLINDRICAL_SURFACE ( 'NONE', #5320, 0.7849999999999991429 ) ;
#2149 = AXIS2_PLACEMENT_3D ( 'NONE', #12762, #11478, #2290 ) ;
#2150 = CARTESIAN_POINT ( 'NONE',  ( 0.3725000000000000533, 0.000000000000000000, 0.4124999999999999778 ) ) ;
#2151 = ORIENTED_EDGE ( 'NONE', *, *, #793, .F. ) ;
#2152 = DIRECTION ( 'NONE',  ( 0.000000000000000000, 0.000000000000000000, -1.000000000000000000 ) ) ;
#2153 = CARTESIAN_POINT ( 'NONE',  ( 0.8264518852088634793, -0.4832231282500065728, -0.3598842701486069662 ) ) ;
#2154 = ORIENTED_EDGE ( 'NONE', *, *, #12110, .T. ) ;
#2155 = CONICAL_SURFACE ( 'NONE', #12177, 0.3750000000000007772, 0.7853981633974579379 ) ;
#2156 = DIRECTION ( 'NONE',  ( 0.000000000000000000, 0.000000000000000000, -1.000000000000000000 ) ) ;
#2157 = CARTESIAN_POINT ( 'NONE',  ( 3.874999999999999556, 3.137999999999999901, -1.820000000000000284 ) ) ;
#2158 = ORIENTED_EDGE ( 'NONE', *, *, #9118, .F. ) ;
#2159 = DIRECTION ( 'NONE',  ( 0.000000000000000000, 0.000000000000000000, -1.000000000000000000 ) ) ;
#2160 = ADVANCED_BREP_SHAPE_REPRESENTATION ( '', ( #10609, #5584, #8424 ), #9397 ) ;
#2161 = ADVANCED_FACE ( 'NONE', ( #2694 ), #10732, .T. ) ;
#2162 = EDGE_CURVE ( 'NONE', #436, #9069, #7540, .T. ) ;
#2163 = DIRECTION ( 'NONE',  ( 0.000000000000000000, 0.000000000000000000, -1.000000000000000000 ) ) ;
#2164 = ORIENTED_EDGE ( 'NONE', *, *, #8583, .F. ) ;
#2165 = CARTESIAN_POINT ( 'NONE',  ( 2.650000000000001688, 0.000000000000000000, 0.000000000000000000 ) ) ;
#2166 =( BOUNDED_SURFACE ( )  B_SPLINE_SURFACE ( 3, 2, ( 
 ( #8892, #3080, #4073 ),
 ( #8975, #13617, #13386 ),
 ( #6675, #9287, #6838 ),
 ( #990, #1067, #12705 ),
 ( #13840, #10340, #4609 ),
 ( #5680, #3382, #15082 ),
 ( #13922, #9120, #15002 ),
 ( #2146, #4530, #7974 ),
 ( #8135, #11563, #9201 ),
 ( #3458, #2230, #8063 ) ),
 .UNSPECIFIED., .F., .F., .F. ) 
 B_SPLINE_SURFACE_WITH_KNOTS ( ( 4, 2, 2, 2, 4 ),
 ( 3, 3 ),
 ( 0.7853981633974539411, 0.9730210579868447951, 1.160643952576235760, 1.348266847165626725, 1.535889741755017690 ),
 ( 0.000000000000000000, 1.000000000000000000 ),
 .UNSPECIFIED. ) 
 GEOMETRIC_REPRESENTATION_ITEM ( )  RATIONAL_B_SPLINE_SURFACE ( (
 ( 1.000000000000000000, 0.7106287314217426543, 1.000000000000000000),
 ( 1.000000000000000000, 0.7104090318602969134, 1.000000000000000000),
 ( 1.000000000000000000, 0.7101685202378590356, 1.000000000000000000),
 ( 1.000000000000000000, 0.7096543062750036990, 1.000000000000000000),
 ( 1.000000000000000000, 0.7093805931376407914, 1.000000000000000000),
 ( 1.000000000000000000, 0.7088094415865170417, 1.000000000000000000),
 ( 1.000000000000000000, 0.7085120144470745673, 1.000000000000000000),
 ( 1.000000000000000000, 0.7079038033994521362, 1.000000000000000000),
 ( 1.000000000000000000, 0.7075930366720840636, 1.000000000000000000),
 ( 1.000000000000000000, 0.7072810196742753686, 1.000000000000000000) ) ) 
 REPRESENTATION_ITEM ( '' )  SURFACE ( )  );
#2167 = AXIS2_PLACEMENT_3D ( 'NONE', #13845, #7981, #12776 ) ;
#2168 = VECTOR ( 'NONE', #1532, 39.37007874015748143 ) ;
#2169 = FACE_OUTER_BOUND ( 'NONE', #6885, .T. ) ;
#2170 = DIRECTION ( 'NONE',  ( -1.000000000000000000, -0.000000000000000000, -0.000000000000000000 ) ) ;
#2171 = AXIS2_PLACEMENT_3D ( 'NONE', #10846, #5045, #8566 ) ;
#2172 = CIRCLE ( 'NONE', #10741, 0.4999999999999997224 ) ;
#2173 = LINE ( 'NONE', #11890, #13616 ) ;
#2174 = CARTESIAN_POINT ( 'NONE',  ( 8.850000000000576961, 0.8820000000023067166, 0.04908333765188085257 ) ) ;
#2175 = AXIS2_PLACEMENT_3D ( 'NONE', #95, #3994, #9312 ) ;
#2176 = CARTESIAN_POINT ( 'NONE',  ( 3.934394892992688408, 1.784885785108176748, -0.7480858108736904155 ) ) ;
#2177 = ORIENTED_EDGE ( 'NONE', *, *, #12261, .T. ) ;
#2178 = VERTEX_POINT ( 'NONE', #13297 ) ;
#2179 = CIRCLE ( 'NONE', #944, 1.000000000000000000 ) ;
#2180 = EDGE_CURVE ( 'NONE', #14371, #9069, #3843, .T. ) ;
#2181 = LINE ( 'NONE', #13437, #7472 ) ;
#2182 = EDGE_LOOP ( 'NONE', ( #1514, #7402, #9942, #283 ) ) ;
#2183 = CARTESIAN_POINT ( 'NONE',  ( 0.4274235469976374047, 1.569496918332969226, -0.02158620620081013602 ) ) ;
#2184 = EDGE_CURVE ( 'NONE', #8852, #2297, #5354, .T. ) ;
#2185 = DIRECTION ( 'NONE',  ( 0.000000000000000000, 0.000000000000000000, -1.000000000000000000 ) ) ;
#2186 = CARTESIAN_POINT ( 'NONE',  ( 2.087921535706059650, 0.2870784642939424591, -0.4105035982572216025 ) ) ;
#2187 = CYLINDRICAL_SURFACE ( 'NONE', #5589, 0.5000000000000002220 ) ;
#2188 = VERTEX_POINT ( 'NONE', #5069 ) ;
#2189 = CARTESIAN_POINT ( 'NONE',  ( 3.128620250494149158, 2.499382783242935169, -0.05744091823031614169 ) ) ;
#2190 = CARTESIAN_POINT ( 'NONE',  ( 0.6555160077358781479, -0.04016535781661281779, -0.5098802871450590635 ) ) ;
#2191 = LINE ( 'NONE', #5339, #14425 ) ;
#2192 = VECTOR ( 'NONE', #7593, 39.37007874015748854 ) ;
#2193 = FACE_OUTER_BOUND ( 'NONE', #8185, .T. ) ;
#2194 = CARTESIAN_POINT ( 'NONE',  ( 4.614277204963975976, 1.747273315043324615, -0.1397865401030924659 ) ) ;
#2195 = EDGE_CURVE ( 'NONE', #587, #9577, #11716, .T. ) ;
#2196 = ORIENTED_EDGE ( 'NONE', *, *, #11253, .F. ) ;
#2198 = EDGE_LOOP ( 'NONE', ( #1788, #15041, #6470, #8160 ) ) ;
#2197 = CARTESIAN_POINT ( 'NONE',  ( 2.774999999999999911, -2.360000000000016751, -1.574999999999999956 ) ) ;
#2199 = EDGE_LOOP ( 'NONE', ( #2971, #11575 ) ) ;
#2201 = VERTEX_POINT ( 'NONE', #1376 ) ;
#2200 = PLANE ( 'NONE',  #7013 ) ;
#2202 = ORIENTED_EDGE ( 'NONE', *, *, #6153, .T. ) ;
#2203 = LINE ( 'NONE', #6887, #1139 ) ;
#2204 =( CONVERSION_BASED_UNIT ( 'INCH', #15136 ) LENGTH_UNIT ( ) NAMED_UNIT ( #1565 ) );
#2205 = DIRECTION ( 'NONE',  ( 0.000000000000000000, 0.000000000000000000, -1.000000000000000000 ) ) ;
#2206 = ORIENTED_EDGE ( 'NONE', *, *, #13800, .T. ) ;
#2207 = LINE ( 'NONE', #7874, #12820 ) ;
#2208 = CARTESIAN_POINT ( 'NONE',  ( 2.774999999999999911, 2.400000000000011458, 0.6999999999999614309 ) ) ;
#2209 = CARTESIAN_POINT ( 'NONE',  ( 3.874999999999999556, 3.137999999999999901, 1.098000000000000087 ) ) ;
#2210 = CARTESIAN_POINT ( 'NONE',  ( 2.774999999999999911, -1.679378605318059048, -1.384878605318056399 ) ) ;
#2211 = FACE_OUTER_BOUND ( 'NONE', #7377, .T. ) ;
#2212 = AXIS2_PLACEMENT_3D ( 'NONE', #11604, #7111, #182 ) ;
#2213 = CARTESIAN_POINT ( 'NONE',  ( 3.063895178286538457, 1.056999999999999496, 0.3964908961568774926 ) ) ;
#2214 = CARTESIAN_POINT ( 'NONE',  ( 2.774999999999999911, -0.6999999999999990674, -2.399999999999999911 ) ) ;
#2215 = FACE_OUTER_BOUND ( 'NONE', #1978, .T. ) ;
#2216 = CARTESIAN_POINT ( 'NONE',  ( 2.774999999999999911, 1.575000000000000178, -2.360000000000018971 ) ) ;
#2217 = EDGE_CURVE ( 'NONE', #13066, #14804, #443, .T. ) ;
#2218 = CARTESIAN_POINT ( 'NONE',  ( 0.000000000000000000, 0.000000000000000000, 0.000000000000000000 ) ) ;
#2219 = EDGE_CURVE ( 'NONE', #13739, #7714, #4921, .T. ) ;
#2220 = ADVANCED_FACE ( 'NONE', ( #9589 ), #13157, .F. ) ;
#2221 = CARTESIAN_POINT ( 'NONE',  ( 3.394491571325182644, 1.679378605318042395, -1.941878605318058337 ) ) ;
#2223 = EDGE_LOOP ( 'NONE', ( #3449, #14253, #4944, #6407 ) ) ;
#2222 = FACE_BOUND ( 'NONE', #13286, .T. ) ;
#2224 = ORIENTED_EDGE ( 'NONE', *, *, #4492, .F. ) ;
#2225 = DIRECTION ( 'NONE',  ( -0.01412288512831583534, 0.000000000000000000, 0.9999002670844989726 ) ) ;
#2226 = ORIENTED_EDGE ( 'NONE', *, *, #5942, .T. ) ;
#2227 = AXIS2_PLACEMENT_3D ( 'NONE', #2077, #6766, #5623 ) ;
#2228 = DIRECTION ( 'NONE',  ( 8.659560562354900811E-17, -0.7071067811865500152, 0.7071067811865449082 ) ) ;
#2229 = ADVANCED_FACE ( 'NONE', ( #14386 ), #7086, .F. ) ;
#2230 = CARTESIAN_POINT ( 'NONE',  ( 3.391025564058367081, 0.6913684120611767181, -0.4521041586997406325 ) ) ;
#2231 = EDGE_CURVE ( 'NONE', #9631, #11384, #11873, .T. ) ;
#2232 = DIRECTION ( 'NONE',  ( -1.000000000000000000, -0.000000000000000000, -0.000000000000000000 ) ) ;
#2233 = DIRECTION ( 'NONE',  ( 0.000000000000000000, -1.000000000000000000, 0.000000000000000000 ) ) ;
#2234 = EDGE_LOOP ( 'NONE', ( #3808, #13892, #8557, #11658, #11611 ) ) ;
#2235 = CARTESIAN_POINT ( 'NONE',  ( 3.369979506347997589, 1.982223984522141658, -0.6498426228982311370 ) ) ;
#2236 = AXIS2_PLACEMENT_3D ( 'NONE', #7902, #9062, #10207 ) ;
#2237 = DIRECTION ( 'NONE',  ( 0.000000000000000000, -1.000000000000000000, 0.000000000000000000 ) ) ;
#2238 = ORIENTED_EDGE ( 'NONE', *, *, #3192, .F. ) ;
#2239 = CARTESIAN_POINT ( 'NONE',  ( 3.394491571325180423, -1.679378605318059048, -1.941878605318027251 ) ) ;
#2240 = ORIENTED_EDGE ( 'NONE', *, *, #12623, .T. ) ;
#2241 = CYLINDRICAL_SURFACE ( 'NONE', #6632, 0.2625000000000000111 ) ;
#2242 = CARTESIAN_POINT ( 'NONE',  ( 2.124999999999999556, 2.360000000000016307, 0.9799999999999454703 ) ) ;
#2243 = EDGE_LOOP ( 'NONE', ( #12112, #620, #6494, #2715 ) ) ;
#2244 = ADVANCED_FACE ( 'NONE', ( #12018 ), #8584, .F. ) ;
#2245 = CARTESIAN_POINT ( 'NONE',  ( 0.7849999999999999201, -0.4829999999999998739, -0.3750000000000000555 ) ) ;
#2246 = AXIS2_PLACEMENT_3D ( 'NONE', #4092, #9760, #13253 ) ;
#2247 = CARTESIAN_POINT ( 'NONE',  ( 1.000048944713735732, -0.4428998280398802612, -0.4293350073753851581 ) ) ;
#2248 = EDGE_CURVE ( 'NONE', #11406, #13592, #7317, .T. ) ;
#2249 = CARTESIAN_POINT ( 'NONE',  ( 3.572691639587101342, 1.991786753997381032, 0.4009351690867059559 ) ) ;
#2250 = EDGE_CURVE ( 'NONE', #10691, #14656, #2670, .T. ) ;
#2251 = DIRECTION ( 'NONE',  ( 1.000000000000000000, 0.000000000000000000, 0.000000000000000000 ) ) ;
#2252 = CARTESIAN_POINT ( 'NONE',  ( 3.952519222920175324, 1.780293626097628312, -0.7464614403131658582 ) ) ;
#2253 = ORIENTED_EDGE ( 'NONE', *, *, #11960, .T. ) ;
#2254 = ORIENTED_EDGE ( 'NONE', *, *, #10137, .T. ) ;
#2255 = DIRECTION ( 'NONE',  ( -0.000000000000000000, -1.000000000000000000, -0.000000000000000000 ) ) ;
#2256 = ORIENTED_EDGE ( 'NONE', *, *, #12470, .F. ) ;
#2257 = CARTESIAN_POINT ( 'NONE',  ( 0.4150689297652778165, 1.581084130983677838, -0.04298503095532220375 ) ) ;
#2258 = CARTESIAN_POINT ( 'NONE',  ( 0.9057578075688627051, -0.4609683907622129651, -0.4498600698720966462 ) ) ;
#2259 = CYLINDRICAL_SURFACE ( 'NONE', #12422, 0.05999999999999992839 ) ;
#2260 = DIRECTION ( 'NONE',  ( 0.000000000000000000, -1.000000000000000000, 0.000000000000000000 ) ) ;
#2261 = ORIENTED_EDGE ( 'NONE', *, *, #12619, .T. ) ;
#2262 = CARTESIAN_POINT ( 'NONE',  ( 2.774999999999999911, 1.574999999999994849, -1.575000000000022160 ) ) ;
#2263 = CARTESIAN_POINT ( 'NONE',  ( 0.7058998964907864382, -0.06000000000000039330, -0.4900296624789436950 ) ) ;
#2264 = FACE_OUTER_BOUND ( 'NONE', #6706, .T. ) ;
#2265 = EDGE_CURVE ( 'NONE', #4893, #9885, #11208, .T. ) ;
#2266 = DIRECTION ( 'NONE',  ( 1.000000000000000000, 0.000000000000000000, 0.000000000000000000 ) ) ;
#2267 = CARTESIAN_POINT ( 'NONE',  ( 4.623972717631986029, 1.748760572069723906, 0.07156785328136136548 ) ) ;
#2268 = ORIENTED_EDGE ( 'NONE', *, *, #11663, .F. ) ;
#2270 = ORIENTED_EDGE ( 'NONE', *, *, #7729, .T. ) ;
#2269 = CARTESIAN_POINT ( 'NONE',  ( 0.2447605936724075171, 1.581084130983678060, 0.3379677220206893096 ) ) ;
#2271 = ORIENTED_EDGE ( 'NONE', *, *, #11401, .T. ) ;
#2273 = VERTEX_POINT ( 'NONE', #898 ) ;
#2272 = FACE_OUTER_BOUND ( 'NONE', #1787, .T. ) ;
#2274 = ORIENTED_EDGE ( 'NONE', *, *, #14689, .T. ) ;
#2275 = PLANE ( 'NONE',  #3343 ) ;
#2276 = DIRECTION ( 'NONE',  ( 0.9994005049267692398, 1.575508169072536402E-15, 0.03462124711963546903 ) ) ;
#2277 = DIRECTION ( 'NONE',  ( 0.000000000000000000, -1.000000000000000000, 0.000000000000000000 ) ) ;
#2278 = ORIENTED_EDGE ( 'NONE', *, *, #11226, .F. ) ;
#2279 = CIRCLE ( 'NONE', #13019, 0.2225000000000001421 ) ;
#2280 = DIRECTION ( 'NONE',  ( -1.000000000000000000, -0.000000000000000000, -0.000000000000000000 ) ) ;
#2281 = CARTESIAN_POINT ( 'NONE',  ( 0.6592054058138496764, -0.4435989489166642930, -0.4885496069960003629 ) ) ;
#2282 = AXIS2_PLACEMENT_3D ( 'NONE', #8970, #4156, #13459 ) ;
#2283 = DIRECTION ( 'NONE',  ( 0.000000000000000000, -1.000000000000000000, 0.000000000000000000 ) ) ;
#2284 = CLOSED_SHELL ( 'NONE', ( #2636, #14870, #10597, #9330, #454, #1599, #325, #2501, #6550, #5036, #6155, #5956, #10561, #1915, #782 ) ) ;
#2285 = DIRECTION ( 'NONE',  ( -1.000000000000000000, -1.874307916738609066E-16, 0.000000000000000000 ) ) ;
#2286 = EDGE_CURVE ( 'NONE', #3133, #5982, #4216, .T. ) ;
#2287 = FACE_OUTER_BOUND ( 'NONE', #10778, .T. ) ;
#2288 = CARTESIAN_POINT ( 'NONE',  ( 0.9176380235743000213, 0.1749999999999999889, -0.1164708448095589793 ) ) ;
#2289 = LINE ( 'NONE', #4826, #14616 ) ;
#2290 = DIRECTION ( 'NONE',  ( 0.000000000000000000, 0.000000000000000000, 1.000000000000000000 ) ) ;
#2291 = CARTESIAN_POINT ( 'NONE',  ( 3.544764658934682178, 0.9266133244050206441, 0.3767952779536547503 ) ) ;
#2292 = CARTESIAN_POINT ( 'NONE',  ( 4.680957888034550152, 1.732455423116393334, -0.08709515200038929483 ) ) ;
#2293 = AXIS2_PLACEMENT_3D ( 'NONE', #12771, #14073, #4758 ) ;
#2294 = EDGE_LOOP ( 'NONE', ( #2980, #10743, #9660, #12572 ) ) ;
#2295 = CARTESIAN_POINT ( 'NONE',  ( 3.426491571325181340, -0.9799999999999986500, -3.359999999999999876 ) ) ;
#2297 = VERTEX_POINT ( 'NONE', #8877 ) ;
#2296 = CARTESIAN_POINT ( 'NONE',  ( 6.176491571325181340, -1.679378605318048390, 1.272378605318051914 ) ) ;
#2298 = ORIENTED_EDGE ( 'NONE', *, *, #11565, .T. ) ;
#2299 = CYLINDRICAL_SURFACE ( 'NONE', #2293, 3.000000000000000444 ) ;
#2300 = ORIENTED_EDGE ( 'NONE', *, *, #3918, .F. ) ;
#2301 = DIRECTION ( 'NONE',  ( 0.000000000000000000, 0.000000000000000000, 1.000000000000000000 ) ) ;
#2302 = CIRCLE ( 'NONE', #6223, 0.5000000000000001110 ) ;
#2303 = EDGE_CURVE ( 'NONE', #6443, #843, #13521, .T. ) ;
#2304 =( REPRESENTATION_RELATIONSHIP ('NONE','NONE', #3591, #1600 ) REPRESENTATION_RELATIONSHIP_WITH_TRANSFORMATION ( #14810 )SHAPE_REPRESENTATION_RELATIONSHIP( ) );
#2305 = EDGE_CURVE ( 'NONE', #391, #5032, #10730, .T. ) ;
#2306 = LINE ( 'NONE', #220, #3798 ) ;
#2307 = EDGE_CURVE ( 'NONE', #7601, #7622, #8047, .T. ) ;
#2308 = DIRECTION ( 'NONE',  ( -0.000000000000000000, -0.000000000000000000, 1.000000000000000000 ) ) ;
#2309 = VERTEX_POINT ( 'NONE', #14608 ) ;
#2310 = CARTESIAN_POINT ( 'NONE',  ( 3.389094372952905942, 2.001744261784617951, -0.5707014325286834389 ) ) ;
#2311 = LINE ( 'NONE', #6993, #3479 ) ;
#2312 = DIRECTION ( 'NONE',  ( -0.000000000000000000, -1.000000000000000000, 0.000000000000000000 ) ) ;
#2313 = EDGE_LOOP ( 'NONE', ( #10259, #11212, #13436, #962 ) ) ;
#2314 = ADVANCED_FACE ( 'NONE', ( #2918 ), #3656, .F. ) ;
#2315 = CONICAL_SURFACE ( 'NONE', #3040, 1.000000000000000000, 0.7853981633974488341 ) ;
#2316 = DIRECTION ( 'NONE',  ( 0.000000000000000000, 0.000000000000000000, 1.000000000000000000 ) ) ;
#2317 = ORIENTED_EDGE ( 'NONE', *, *, #10964, .F. ) ;
#2318 = CARTESIAN_POINT ( 'NONE',  ( 3.426491571325181340, 1.679378605318059048, 1.679378605318041506 ) ) ;
#2319 = AXIS2_PLACEMENT_3D ( 'NONE', #14710, #10201, #3311 ) ;
#2320 = CIRCLE ( 'NONE', #6720, 0.2812500000000000555 ) ;
#2321 = DIRECTION ( 'NONE',  ( -0.000000000000000000, -1.000000000000000000, -0.000000000000000000 ) ) ;
#2322 = EDGE_LOOP ( 'NONE', ( #5269, #8774, #15052, #5211 ) ) ;
#2323 = CARTESIAN_POINT ( 'NONE',  ( 6.208491571325183145, 1.679378605318035733, -1.679378605318065487 ) ) ;
#2324 = CARTESIAN_POINT ( 'NONE',  ( 2.806999999999999940, -1.679378605318059048, -1.679378605318041950 ) ) ;
#2325 = AXIS2_PLACEMENT_3D ( 'NONE', #9410, #4899, #1124 ) ;
#2326 = DIRECTION ( 'NONE',  ( 1.000000000000000000, 0.000000000000000000, 0.000000000000000000 ) ) ;
#2327 = CONICAL_SURFACE ( 'NONE', #1338, 1.932031071636253650, 0.2617993877991429685 ) ;
#2328 = AXIS2_PLACEMENT_3D ( 'NONE', #5829, #10414, #5906 ) ;
#2329 = CARTESIAN_POINT ( 'NONE',  ( 0.06299999999999994493, 0.000000000000000000, 0.000000000000000000 ) ) ;
#2330 = CARTESIAN_POINT ( 'NONE',  ( 3.598300749230342710, 1.876349019058903611, -0.7608587385032532513 ) ) ;
#2331 = EDGE_LOOP ( 'NONE', ( #667, #4379, #10792, #5951 ) ) ;
#2332 = VERTEX_POINT ( 'NONE', #11088 ) ;
#2333 = EDGE_CURVE ( 'NONE', #2708, #11839, #3893, .T. ) ;
#2334 = AXIS2_PLACEMENT_3D ( 'NONE', #12175, #10882, #9963 ) ;
#2335 = CARTESIAN_POINT ( 'NONE',  ( 1.003096136995459631, -0.4429976034824900655, -0.4258273028168327867 ) ) ;
#2336 = ORIENTED_EDGE ( 'NONE', *, *, #14156, .T. ) ;
#2337 = DIRECTION ( 'NONE',  ( 0.000000000000000000, 0.000000000000000000, -1.000000000000000000 ) ) ;
#2338 = AXIS2_PLACEMENT_3D ( 'NONE', #12524, #12752, #2041 ) ;
#2339 = CIRCLE ( 'NONE', #2348, 0.07999999999999996003 ) ;
#2340 = CARTESIAN_POINT ( 'NONE',  ( 0.9575621992971196095, -0.4805093615874324597, -0.4235284989533516509 ) ) ;
#2341 = ADVANCED_FACE ( 'NONE', ( #666 ), #7798, .F. ) ;
#2342 = CYLINDRICAL_SURFACE ( 'NONE', #4115, 0.03999999999999998002 ) ;
#2343 = ORIENTED_EDGE ( 'NONE', *, *, #12948, .T. ) ;
#2344 = CARTESIAN_POINT ( 'NONE',  ( -0.4124999999999999223, 0.000000000000000000, 0.3724999999999999978 ) ) ;
#2345 = CARTESIAN_POINT ( 'NONE',  ( 1.002120845300913610, -0.4429991133026480732, -0.4270309162001265646 ) ) ;
#2346 = CARTESIAN_POINT ( 'NONE',  ( 2.774999999999999911, -1.679378605318059048, -1.679378605318041950 ) ) ;
#2347 = AXIS2_PLACEMENT_3D ( 'NONE', #12245, #2845, #1754 ) ;
#2348 = AXIS2_PLACEMENT_3D ( 'NONE', #10790, #9789, #2825 ) ;
#2349 = CARTESIAN_POINT ( 'NONE',  ( -1.152890932057317374E-17, -0.4429999999999998939, -0.5000000000000000000 ) ) ;
#2350 = CARTESIAN_POINT ( 'NONE',  ( 4.623480434945832052, 1.809913863617587104, -0.07025183563157885724 ) ) ;
#2351 = ORIENTED_EDGE ( 'NONE', *, *, #4610, .F. ) ;
#2353 = ORIENTED_EDGE ( 'NONE', *, *, #7924, .T. ) ;
#2352 = DIRECTION ( 'NONE',  ( -1.000000000000000000, -0.000000000000000000, -0.000000000000000000 ) ) ;
#2354 =( REPRESENTATION_RELATIONSHIP ('NONE','NONE', #3591, #8297 ) REPRESENTATION_RELATIONSHIP_WITH_TRANSFORMATION ( #14577 )SHAPE_REPRESENTATION_RELATIONSHIP( ) );
#2355 = ORIENTED_EDGE ( 'NONE', *, *, #5210, .F. ) ;
#2357 = VERTEX_POINT ( 'NONE', #12838 ) ;
#2356 = LINE ( 'NONE', #6032, #10422 ) ;
#2358 = ORIENTED_EDGE ( 'NONE', *, *, #6508, .F. ) ;
#2359 = EDGE_CURVE ( 'NONE', #2844, #587, #14385, .T. ) ;
#2360 = DIRECTION ( 'NONE',  ( 0.000000000000000000, 0.000000000000000000, -1.000000000000000000 ) ) ;
#2361 = EDGE_CURVE ( 'NONE', #13169, #10530, #11713, .T. ) ;
#2362 = AXIS2_PLACEMENT_3D ( 'NONE', #2826, #10862, #11154 ) ;
#2363 = DIRECTION ( 'NONE',  ( -1.365923996832131609E-16, 1.000000000000000000, -0.000000000000000000 ) ) ;
#2364 = EDGE_LOOP ( 'NONE', ( #11571, #13014, #9703, #3204 ) ) ;
#2365 = CARTESIAN_POINT ( 'NONE',  ( 2.774999999999999911, 1.679378605318042395, -1.679378605318058604 ) ) ;
#2366 = DIRECTION ( 'NONE',  ( 0.7071067811865487940, 0.7071067811865461294, 0.000000000000000000 ) ) ;
#2367 = CARTESIAN_POINT ( 'NONE',  ( 0.7500000000000001110, 1.000000000000000000, 0.6614378277661475680 ) ) ;
#2368 = VECTOR ( 'NONE', #10171, 39.37007874015748143 ) ;
#2369 = CARTESIAN_POINT ( 'NONE',  ( 6.176491571325181340, -1.679378605318048390, 2.086378605318056412 ) ) ;
#2370 = LINE ( 'NONE', #7048, #9195 ) ;
#2371 = DIRECTION ( 'NONE',  ( 0.000000000000000000, 0.000000000000000000, -1.000000000000000000 ) ) ;
#2372 = AXIS2_PLACEMENT_3D ( 'NONE', #10839, #11055, #553 ) ;
#2373 = DIRECTION ( 'NONE',  ( 0.000000000000000000, 0.000000000000000000, -1.000000000000000000 ) ) ;
#2374 = CARTESIAN_POINT ( 'NONE',  ( 3.610061643217520988, 0.9055534390348793927, 0.4243489690802683678 ) ) ;
#2375 = CARTESIAN_POINT ( 'NONE',  ( 4.431846745274908628, 1.707674138507286443, 0.5735374726554932634 ) ) ;
#2376 = ORIENTED_EDGE ( 'NONE', *, *, #12242, .T. ) ;
#2377 = CARTESIAN_POINT ( 'NONE',  ( 3.426491571325181340, -1.679378605318041950, 1.679378605318059048 ) ) ;
#2378 = VECTOR ( 'NONE', #11522, 39.37007874015748143 ) ;
#2380 = VERTEX_POINT ( 'NONE', #3364 ) ;
#2379 = CARTESIAN_POINT ( 'NONE',  ( -0.4125000000000000333, -0.6590000000000000302, 0.4124999999999999223 ) ) ;
#2381 = EDGE_LOOP ( 'NONE', ( #6537, #1267 ) ) ;
#2382 = DIRECTION ( 'NONE',  ( -1.000000000000000000, 0.000000000000000000, 0.000000000000000000 ) ) ;
#2383 = FACE_OUTER_BOUND ( 'NONE', #14366, .T. ) ;
#2384 = ORIENTED_EDGE ( 'NONE', *, *, #12791, .T. ) ;
#2385 = DIRECTION ( 'NONE',  ( -0.000000000000000000, -1.000000000000000000, -0.000000000000000000 ) ) ;
#2386 = VECTOR ( 'NONE', #6238, 39.37007874015748143 ) ;
#2387 = DIRECTION ( 'NONE',  ( 0.000000000000000000, -0.000000000000000000, -1.000000000000000000 ) ) ;
#2388 = DIRECTION ( 'NONE',  ( 0.000000000000000000, 0.000000000000000000, -1.000000000000000000 ) ) ;
#2389 = CIRCLE ( 'NONE', #12879, 0.06000000000000001166 ) ;
#2390 = ORIENTED_EDGE ( 'NONE', *, *, #3595, .T. ) ;
#2391 = CARTESIAN_POINT ( 'NONE',  ( 0.7007157546338583787, -0.4033010131257052655, 0.4867155808989060417 ) ) ;
#2392 = CARTESIAN_POINT ( 'NONE',  ( 3.599851685419308556, 0.9969999999999999973, 0.3891486526398028056 ) ) ;
#2393 = DIRECTION ( 'NONE',  ( 8.659560562354816994E-17, -0.7071067811865568986, 0.7071067811865381358 ) ) ;
#2394 = ORIENTED_EDGE ( 'NONE', *, *, #2726, .F. ) ;
#2395 = DIRECTION ( 'NONE',  ( 8.659560562354959975E-17, -0.7071067811865452413, 0.7071067811865496822 ) ) ;
#2396 = VERTEX_POINT ( 'NONE', #3288 ) ;
#2397 = EDGE_CURVE ( 'NONE', #14837, #6053, #1131, .T. ) ;
#2398 = TOROIDAL_SURFACE ( 'NONE', #3129, 0.7173254825712083171, 0.05999999999999999778 ) ;
#2399 = CARTESIAN_POINT ( 'NONE',  ( 4.344846310392954436, 2.750000000000000000, -1.491010071662831171 ) ) ;
#2400 = VERTEX_POINT ( 'NONE', #4441 ) ;
#2401 = AXIS2_PLACEMENT_3D ( 'NONE', #7870, #6806, #5431 ) ;
#2402 = CYLINDRICAL_SURFACE ( 'NONE', #6006, 0.1899999999999996136 ) ;
#2403 = CARTESIAN_POINT ( 'NONE',  ( 2.372634528609594007, 0.1852128444980911670, -0.4664882128727459998 ) ) ;
#2404 = AXIS2_PLACEMENT_3D ( 'NONE', #8879, #3065, #14917 ) ;
#2405 = ADVANCED_FACE ( 'NONE', ( #13979 ), #13907, .F. ) ;
#2406 = CARTESIAN_POINT ( 'NONE',  ( 2.124999999999999556, 1.679378605318042395, -1.384878605318058842 ) ) ;
#2407 = CIRCLE ( 'NONE', #6073, 0.2219999999999999751 ) ;
#2408 = AXIS2_PLACEMENT_3D ( 'NONE', #218, #13076, #2757 ) ;
#2409 = CARTESIAN_POINT ( 'NONE',  ( 0.2099999999999999922, 1.559103846021543172, -0.3809527529760087239 ) ) ;
#2410 = VECTOR ( 'NONE', #2308, 39.37007874015748143 ) ;
#2411 = CARTESIAN_POINT ( 'NONE',  ( 3.952950666365288690, 1.759291877752760414, -0.7927856782489325349 ) ) ;
#2412 = ORIENTED_EDGE ( 'NONE', *, *, #9018, .F. ) ;
#2413 = EDGE_CURVE ( 'NONE', #1037, #8543, #14096, .T. ) ;
#2414 = AXIS2_PLACEMENT_3D ( 'NONE', #8588, #6144, #14390 ) ;
#2415 = EDGE_LOOP ( 'NONE', ( #3462, #6075, #12152, #11692 ) ) ;
#2416 = CARTESIAN_POINT ( 'NONE',  ( 0.06299999999999994493, 3.000000000000000444, 0.000000000000000000 ) ) ;
#2417 = ORIENTED_EDGE ( 'NONE', *, *, #627, .T. ) ;
#2418 = EDGE_CURVE ( 'NONE', #14846, #14201, #852, .T. ) ;
#2419 = COLOUR_RGB ( '',0.7921568627450980005, 0.8196078431372548767, 0.9333333333333333481 ) ;
#2420 = DIRECTION ( 'NONE',  ( -1.874307916738606601E-16, 1.000000000000000000, 0.000000000000000000 ) ) ;
#2421 = CARTESIAN_POINT ( 'NONE',  ( 3.426491571325181340, 0.9799999999999438050, -2.360000000000016307 ) ) ;
#2423 = CYLINDRICAL_SURFACE ( 'NONE', #4885, 0.8000000000000000444 ) ;
#2422 = VECTOR ( 'NONE', #14735, 39.37007874015748143 ) ;
#2424 = CARTESIAN_POINT ( 'NONE',  ( 0.7034818293080734586, -0.02506196876506533791, -0.4790337915202405039 ) ) ;
#2425 = VERTEX_POINT ( 'NONE', #53 ) ;
#2426 = AXIS2_PLACEMENT_3D ( 'NONE', #9931, #5417, #1958 ) ;
#2427 = LINE ( 'NONE', #99, #213 ) ;
#2428 = ADVANCED_FACE ( 'NONE', ( #11476 ), #2599, .T. ) ;
#2429 = CARTESIAN_POINT ( 'NONE',  ( 1.328406321535844592, -0.06000000000013446660, 0.4812371988483637453 ) ) ;
#2430 = DIRECTION ( 'NONE',  ( -0.8660254037844328234, 0.000000000000000000, 0.5000000000000101030 ) ) ;
#2431 = ADVANCED_FACE ( 'NONE', ( #10325 ), #2130, .T. ) ;
#2432 = AXIS2_PLACEMENT_3D ( 'NONE', #5872, #7378, #3571 ) ;
#2433 = PLANE ( 'NONE',  #2484 ) ;
#2434 = AXIS2_PLACEMENT_3D ( 'NONE', #3654, #14033, #7175 ) ;
#2435 = CARTESIAN_POINT ( 'NONE',  ( 2.774999999999999911, 1.679378605318042395, -1.679378605318058604 ) ) ;
#2436 = CARTESIAN_POINT ( 'NONE',  ( 4.600670465018250610, 1.805329134815081504, 0.1961885608909609002 ) ) ;
#2437 = ORIENTED_EDGE ( 'NONE', *, *, #7129, .T. ) ;
#2439 = ORIENTED_EDGE ( 'NONE', *, *, #3765, .F. ) ;
#2438 = CARTESIAN_POINT ( 'NONE',  ( 0.4019514777495877822, 1.589927591219149727, 0.06570512431233779815 ) ) ;
#2440 = ORIENTED_EDGE ( 'NONE', *, *, #11014, .F. ) ;
#2441 = DIRECTION ( 'NONE',  ( 0.000000000000000000, 0.000000000000000000, -1.000000000000000000 ) ) ;
#2442 = ORIENTED_EDGE ( 'NONE', *, *, #11847, .F. ) ;
#2443 = CARTESIAN_POINT ( 'NONE',  ( 2.774999999999999911, -2.359999999999979892, 1.575000000000016387 ) ) ;
#2444 = DIRECTION ( 'NONE',  ( -0.000000000000000000, -1.000000000000000000, -0.000000000000000000 ) ) ;
#2445 = ORIENTED_EDGE ( 'NONE', *, *, #6925, .T. ) ;
#2446 = DIRECTION ( 'NONE',  ( 1.000000000000000000, 0.000000000000000000, 0.000000000000000000 ) ) ;
#2447 = EDGE_CURVE ( 'NONE', #14903, #10819, #3568, .T. ) ;
#2448 = DIRECTION ( 'NONE',  ( 0.000000000000000000, 1.000000000000000000, -0.000000000000000000 ) ) ;
#2449 = CARTESIAN_POINT ( 'NONE',  ( 2.742999999999998995, -1.679378605318059048, -1.679378605318041950 ) ) ;
#2450 = CARTESIAN_POINT ( 'NONE',  ( 2.371787155501894784, 0.1852128444980907784, -0.4064941968476759038 ) ) ;
#2451 = CARTESIAN_POINT ( 'NONE',  ( 3.875000000000000000, 3.137999999999999901, 0.000000000000000000 ) ) ;
#2452 = EDGE_CURVE ( 'NONE', #3716, #6251, #7725, .T. ) ;
#2453 = CARTESIAN_POINT ( 'NONE',  ( 3.624016768725874638, 0.9015561565218271900, 0.4327462728766410249 ) ) ;
#2454 = FACE_BOUND ( 'NONE', #7143, .T. ) ;
#2455 = ORIENTED_EDGE ( 'NONE', *, *, #5490, .T. ) ;
#2456 = DIRECTION ( 'NONE',  ( -0.000000000000000000, -1.000000000000000000, 0.000000000000000000 ) ) ;
#2458 = ORIENTED_EDGE ( 'NONE', *, *, #13986, .F. ) ;
#2457 = DIRECTION ( 'NONE',  ( -1.000000000000000000, -0.000000000000000000, -0.000000000000000000 ) ) ;
#2459 = ORIENTED_EDGE ( 'NONE', *, *, #5708, .T. ) ;
#2460 = CARTESIAN_POINT ( 'NONE',  ( 0.8999999999999999112, -0.6429999999999999050, -0.3199999999999985634 ) ) ;
#2461 = DIRECTION ( 'NONE',  ( 0.000000000000000000, 1.000000000000000000, 0.000000000000000000 ) ) ;
#2462 = CARTESIAN_POINT ( 'NONE',  ( 2.683697947871385381, 0.4122708231251925870, 0.4026504426247390356 ) ) ;
#2463 = CIRCLE ( 'NONE', #1465, 0.2224999999999996148 ) ;
#2464 = ORIENTED_EDGE ( 'NONE', *, *, #6240, .F. ) ;
#2465 = CARTESIAN_POINT ( 'NONE',  ( 8.474190026735614722, 1.056999999999999940, 0.3203020658980470503 ) ) ;
#2466 = FACE_OUTER_BOUND ( 'NONE', #5266, .T. ) ;
#2467 = DIRECTION ( 'NONE',  ( 0.000000000000000000, 1.000000000000000000, 0.000000000000000000 ) ) ;
#2468 = ORIENTED_EDGE ( 'NONE', *, *, #15121, .T. ) ;
#2469 = EDGE_CURVE ( 'NONE', #11381, #11962, #12585, .T. ) ;
#2470 = CARTESIAN_POINT ( 'NONE',  ( 3.484027466210578794, 1.954031737839658334, -0.6398539634642703700 ) ) ;
#2471 = PRODUCT_RELATED_PRODUCT_CATEGORY ( 'part', '', ( #9828 ) ) ;
#2472 = PLANE ( 'NONE',  #12506 ) ;
#2473 = CARTESIAN_POINT ( 'NONE',  ( 0.6500000000000001332, 1.679378605318035733, -1.679378605318065487 ) ) ;
#2474 = ORIENTED_EDGE ( 'NONE', *, *, #13056, .T. ) ;
#2475 = CARTESIAN_POINT ( 'NONE',  ( 0.6500000000000001332, 1.679378605318035733, -1.272378605318060796 ) ) ;
#2476 = PRESENTATION_LAYER_ASSIGNMENT (  '', '', ( #4671 ) ) ;
#2477 = CYLINDRICAL_SURFACE ( 'NONE', #5258, 1.000000000000000222 ) ;
#2478 = EDGE_LOOP ( 'NONE', ( #1747, #6310 ) ) ;
#2479 = CARTESIAN_POINT ( 'NONE',  ( 0.09035531712817643224, 1.379999999999999671, 0.1564999999999999447 ) ) ;
#2480 = ORIENTED_EDGE ( 'NONE', *, *, #6699, .T. ) ;
#2481 = DIRECTION ( 'NONE',  ( -0.2588190451024959260, 0.000000000000000000, 0.9659258262890748625 ) ) ;
#2482 = CARTESIAN_POINT ( 'NONE',  ( 1.127821516536288593, -0.3829999999995594151, -0.4840703175630469146 ) ) ;
#2483 = DIRECTION ( 'NONE',  ( 0.000000000000000000, 0.000000000000000000, -1.000000000000000000 ) ) ;
#2484 = AXIS2_PLACEMENT_3D ( 'NONE', #6174, #13115, #2652 ) ;
#2485 = PRODUCT_DEFINITION ( 'UNKNOWN', '', #3289, #1095 ) ;
#2486 = FACE_OUTER_BOUND ( 'NONE', #595, .T. ) ;
#2487 = ORIENTED_EDGE ( 'NONE', *, *, #2947, .F. ) ;
#2488 = EDGE_LOOP ( 'NONE', ( #4732, #7802 ) ) ;
#2489 = VERTEX_POINT ( 'NONE', #4514 ) ;
#2490 = UNCERTAINTY_MEASURE_WITH_UNIT (LENGTH_MEASURE( 1.000000000000000082E-05 ), #14703, 'distance_accuracy_value', 'NONE');
#2491 = CARTESIAN_POINT ( 'NONE',  ( -0.3725000000000002198, 0.2159999999999999698, -0.3725000000000000533 ) ) ;
#2492 = AXIS2_PLACEMENT_3D ( 'NONE', #8925, #13569, #1953 ) ;
#2493 = LINE ( 'NONE', #14027, #389 ) ;
#2494 = CARTESIAN_POINT ( 'NONE',  ( 0.9618064621433325412, -0.4822944676752229931, -0.4180629964233649742 ) ) ;
#2495 = DIRECTION ( 'NONE',  ( -1.000000000000000000, -0.000000000000000000, -0.000000000000000000 ) ) ;
#2496 = EDGE_LOOP ( 'NONE', ( #11790, #11232, #4640, #166 ) ) ;
#2497 = CARTESIAN_POINT ( 'NONE',  ( 3.426491571325181340, 1.987932976489903636, -0.2209981660730357955 ) ) ;
#2498 = CARTESIAN_POINT ( 'NONE',  ( 1.813794508431087138, 0.1486894511060126989, 0.4139507449637807035 ) ) ;
#2499 = CARTESIAN_POINT ( 'NONE',  ( 3.426491571325181340, -1.575000000000027489, -2.359999999999986109 ) ) ;
#2500 = EDGE_CURVE ( 'NONE', #8103, #10897, #11131, .T. ) ;
#2501 = ADVANCED_FACE ( 'NONE', ( #2287 ), #1281, .T. ) ;
#2502 = EDGE_CURVE ( 'NONE', #4426, #8247, #2370, .T. ) ;
#2503 = CARTESIAN_POINT ( 'NONE',  ( 4.532079842494805000, 1.713382837086246058, -0.4627352718838613765 ) ) ;
#2504 = ORIENTED_EDGE ( 'NONE', *, *, #3515, .F. ) ;
#2506 = VERTEX_POINT ( 'NONE', #14915 ) ;
#2505 = CARTESIAN_POINT ( 'NONE',  ( 2.774999999999999911, 3.360000000000016751, 0.9799999999999461364 ) ) ;
#2507 = EDGE_CURVE ( 'NONE', #7355, #13774, #12610, .T. ) ;
#2508 = ADVANCED_FACE ( 'NONE', ( #12692 ), #10784, .T. ) ;
#2509 = ORIENTED_EDGE ( 'NONE', *, *, #3481, .T. ) ;
#2510 = CARTESIAN_POINT ( 'NONE',  ( 0.6179999999999962190, -1.679378605318048390, 1.679378605318054163 ) ) ;
#2511 = ORIENTED_EDGE ( 'NONE', *, *, #11180, .T. ) ;
#2512 = AXIS2_PLACEMENT_3D ( 'NONE', #8729, #3771, #6438 ) ;
#2513 = DIRECTION ( 'NONE',  ( 0.000000000000000000, 0.000000000000000000, 1.000000000000000000 ) ) ;
#2514 = DIRECTION ( 'NONE',  ( 0.000000000000000000, 0.000000000000000000, 1.000000000000000000 ) ) ;
#2515 = DIRECTION ( 'NONE',  ( -1.000000000000000000, -0.000000000000000000, -0.000000000000000000 ) ) ;
#2516 = VERTEX_POINT ( 'NONE', #3750 ) ;
#2517 = CARTESIAN_POINT ( 'NONE',  ( 0.000000000000000000, 0.000000000000000000, 3.000000000000000444 ) ) ;
#2518 = DIRECTION ( 'NONE',  ( 0.000000000000000000, 0.000000000000000000, -1.000000000000000000 ) ) ;
#2519 = CARTESIAN_POINT ( 'NONE',  ( 3.426491571325181340, -2.400000000000011902, -0.6999999999999596545 ) ) ;
#2520 = CARTESIAN_POINT ( 'NONE',  ( -0.3724999999999999423, 0.000000000000000000, 0.3724999999999999978 ) ) ;
#2521 = CARTESIAN_POINT ( 'NONE',  ( 8.475037399843312613, 0.9289129992088663856, 0.3802960819231171463 ) ) ;
#2522 = CIRCLE ( 'NONE', #12040, 0.4070000000000000839 ) ;
#2523 = B_SPLINE_CURVE_WITH_KNOTS ( 'NONE', 3,
 ( #10626, #6267, #10928, #11850, #4904, #9779, #4822, #9492, #14140, #12986, #1352, #9568, #3748, #7704 ),
 .UNSPECIFIED., .F., .F.,
 ( 4, 2, 2, 2, 2, 2, 4 ),
 ( 1.868354362588067661E-17, 0.003338103516181846215, 0.005007155274272739182, 0.006676207032363632582, 0.01001431054854545408, 0.01168336230663636482, 0.01335241406472727557 ),
 .UNSPECIFIED. ) ;
#2524 = DIRECTION ( 'NONE',  ( 0.000000000000000000, 0.000000000000000000, -1.000000000000000000 ) ) ;
#2525 = DIRECTION ( 'NONE',  ( 0.7070715176384863021, 0.7070715176384774203, -0.009986885842351498482 ) ) ;
#2526 = DIRECTION ( 'NONE',  ( -1.000000000000000000, -0.000000000000000000, -0.000000000000000000 ) ) ;
#2527 = EDGE_LOOP ( 'NONE', ( #11052, #3694, #10582, #5196 ) ) ;
#2528 = CONICAL_SURFACE ( 'NONE', #7412, 1.039370078740158965, 0.7853981633974517207 ) ;
#2529 = DIRECTION ( 'NONE',  ( -1.000000000000000000, -0.000000000000000000, 0.000000000000000000 ) ) ;
#2531 = VERTEX_POINT ( 'NONE', #14436 ) ;
#2530 = CARTESIAN_POINT ( 'NONE',  ( 4.769268701363833074, 3.567999999999999616, -0.3249191361593797289 ) ) ;
#2532 = ORIENTED_EDGE ( 'NONE', *, *, #9832, .F. ) ;
#2533 = EDGE_CURVE ( 'NONE', #5850, #2201, #6749, .T. ) ;
#2534 = CARTESIAN_POINT ( 'NONE',  ( 2.980731298636167370, 3.137999999999999901, -0.3249191361593797844 ) ) ;
#2535 = DIRECTION ( 'NONE',  ( 0.000000000000000000, -1.000000000000000000, 0.000000000000000000 ) ) ;
#2536 = VERTEX_POINT ( 'NONE', #7486 ) ;
#2537 = CARTESIAN_POINT ( 'NONE',  ( 0.9666441941723522557, -0.4829990576375862155, -0.4094325616265704348 ) ) ;
#2538 = EDGE_CURVE ( 'NONE', #9885, #4893, #123, .T. ) ;
#2539 = DIRECTION ( 'NONE',  ( 1.000000000000000000, 0.000000000000000000, 0.000000000000000000 ) ) ;
#2540 = CIRCLE ( 'NONE', #6947, 0.1249999999999999861 ) ;
#2541 = DIRECTION ( 'NONE',  ( 1.000000000000000000, 0.000000000000000000, 0.000000000000000000 ) ) ;
#2542 = CIRCLE ( 'NONE', #302, 0.3750000000000004996 ) ;
#2543 = EDGE_LOOP ( 'NONE', ( #11950, #526, #292, #6137 ) ) ;
#2544 = DIRECTION ( 'NONE',  ( 0.000000000000000000, 0.000000000000000000, 1.000000000000000000 ) ) ;
#2545 = CARTESIAN_POINT ( 'NONE',  ( 0.7070627455984153098, -0.4242534173714980206, 0.4737642524341733608 ) ) ;
#2546 = DIRECTION ( 'NONE',  ( 0.000000000000000000, 0.000000000000000000, -1.000000000000000000 ) ) ;
#2547 = DIRECTION ( 'NONE',  ( 0.000000000000000000, 0.000000000000000000, 1.000000000000000000 ) ) ;
#2548 = ORIENTED_EDGE ( 'NONE', *, *, #4519, .T. ) ;
#2549 = DIRECTION ( 'NONE',  ( 0.000000000000000000, 0.000000000000000000, 1.000000000000000000 ) ) ;
#2550 = ORIENTED_EDGE ( 'NONE', *, *, #11021, .T. ) ;
#2551 = DIRECTION ( 'NONE',  ( -0.000000000000000000, 1.000000000000000000, -0.000000000000000000 ) ) ;
#2552 = EDGE_LOOP ( 'NONE', ( #13847, #13027, #9844, #2000 ) ) ;
#2553 = AXIS2_PLACEMENT_3D ( 'NONE', #6742, #14695, #748 ) ;
#2554 = CIRCLE ( 'NONE', #13038, 0.07000000000000047851 ) ;
#2555 = DIRECTION ( 'NONE',  ( -1.000000000000000000, -0.000000000000000000, -0.000000000000000000 ) ) ;
#2556 = EDGE_CURVE ( 'NONE', #1593, #6459, #3825, .T. ) ;
#2557 = ADVANCED_FACE ( 'NONE', ( #3964, #7347, #9712, #1438, #1508, #419 ), #203, .T. ) ;
#2558 = DIRECTION ( 'NONE',  ( 0.000000000000000000, 0.000000000000000000, -1.000000000000000000 ) ) ;
#2559 = CARTESIAN_POINT ( 'NONE',  ( 2.045495128834867060, 0.3295048711651353268, 0.5000000000000000000 ) ) ;
#2560 = B_SPLINE_CURVE_WITH_KNOTS ( 'NONE', 3,
 ( #8847, #1952, #3112, #3189 ),
 .UNSPECIFIED., .F., .F.,
 ( 4, 4 ),
 ( 0.01473257324215802161, 0.01653313341413566867 ),
 .UNSPECIFIED. ) ;
#2561 = AXIS2_PLACEMENT_3D ( 'NONE', #8508, #216, #1369 ) ;
#2562 = CARTESIAN_POINT ( 'NONE',  ( -0.4124999999999999223, 0.1749999999999999889, -0.3724999999999999978 ) ) ;
#2563 = ORIENTED_EDGE ( 'NONE', *, *, #11459, .F. ) ;
#2564 = VERTEX_POINT ( 'NONE', #9641 ) ;
#2565 = ORIENTED_EDGE ( 'NONE', *, *, #10757, .F. ) ;
#2566 = DIRECTION ( 'NONE',  ( -1.325335837957478697E-16, 0.7071067811865353603, -0.7071067811865596742 ) ) ;
#2567 = CARTESIAN_POINT ( 'NONE',  ( 0.6179999999999962190, -1.679378605318048390, 1.304378605318053497 ) ) ;
#2568 = CARTESIAN_POINT ( 'NONE',  ( 4.315797241329101475, 2.750000000000000000, 1.570821732971949825 ) ) ;
#2569 = DIRECTION ( 'NONE',  ( -1.000000000000000000, -0.000000000000000000, -0.000000000000000000 ) ) ;
#2570 = ORIENTED_EDGE ( 'NONE', *, *, #6153, .F. ) ;
#2571 = ADVANCED_FACE ( 'NONE', ( #6192 ), #2085, .T. ) ;
#2572 = CARTESIAN_POINT ( 'NONE',  ( 0.7983174577546989781, -0.4429999999999998939, -0.4287183451209413132 ) ) ;
#2573 = VECTOR ( 'NONE', #2481, 39.37007874015748854 ) ;
#2574 = CONICAL_SURFACE ( 'NONE', #1818, 1.875000000000000000, 0.7853981633974482790 ) ;
#2575 = CARTESIAN_POINT ( 'NONE',  ( 1.398131049395755277, 0.007369456331732793068, 0.4802523863079456445 ) ) ;
#2576 =( BOUNDED_SURFACE ( )  B_SPLINE_SURFACE ( 3, 2, ( 
 ( #14145, #3679, #2521 ),
 ( #7199, #6045, #4905 ),
 ( #9571, #2601, #7273 ),
 ( #4269, #2966, #4037 ),
 ( #7706, #12646, #4116 ),
 ( #2891, #3124, #1798 ),
 ( #5186, #7627, #5420 ),
 ( #1013, #12287, #8704 ),
 ( #12367, #2174, #8787 ),
 ( #7558, #7998, #6488 ) ),
 .UNSPECIFIED., .F., .F., .F. ) 
 B_SPLINE_SURFACE_WITH_KNOTS ( ( 4, 2, 2, 2, 4 ),
 ( 3, 3 ),
 ( 4.726512335037234891, 5.115680578072822726, 5.504848821108410561, 5.894017064143998397, 6.283185307179586232 ),
 ( 0.000000000000000000, 1.000000000000000000 ),
 .UNSPECIFIED. ) 
 GEOMETRIC_REPRESENTATION_ITEM ( )  RATIONAL_B_SPLINE_SURFACE ( (
 ( 1.000000000000000000, 0.7072810196742753686, 1.000000000000000000),
 ( 1.000000000000000000, 0.7088814831346345047, 1.000000000000000000),
 ( 1.000000000000000000, 0.7104704279345043227, 1.000000000000000000),
 ( 1.000000000000000000, 0.7133949008902312761, 1.000000000000000000),
 ( 1.000000000000000000, 0.7147290448012498798, 1.000000000000000000),
 ( 1.000000000000000000, 0.7169492149879285181, 1.000000000000000000),
 ( 1.000000000000000000, 0.7178345465032397454, 1.000000000000000000),
 ( 1.000000000000000000, 0.7190300160696035947, 1.000000000000000000),
 ( 1.000000000000000000, 0.7193411551263462211, 1.000000000000000000),
 ( 1.000000000000000000, 0.7193398003386451967, 1.000000000000000000) ) ) 
 REPRESENTATION_ITEM ( '' )  SURFACE ( )  );
#2577 = DIRECTION ( 'NONE',  ( -1.000000000000000000, -0.000000000000000000, -0.000000000000000000 ) ) ;
#2578 = CIRCLE ( 'NONE', #3802, 0.6412116890856960350 ) ;
#2579 = CARTESIAN_POINT ( 'NONE',  ( 4.339042227135573526, 1.728400208608292576, -0.5915559626296543749 ) ) ;
#2580 = ORIENTED_EDGE ( 'NONE', *, *, #11422, .T. ) ;
#2581 = CIRCLE ( 'NONE', #11123, 0.3750000000000004996 ) ;
#2583 = VERTEX_POINT ( 'NONE', #6271 ) ;
#2582 = DIRECTION ( 'NONE',  ( -1.000000000000000000, -0.000000000000000000, -0.000000000000000000 ) ) ;
#2584 = AXIS2_PLACEMENT_3D ( 'NONE', #555, #1643, #10921 ) ;
#2585 = ORIENTED_EDGE ( 'NONE', *, *, #11187, .F. ) ;
#2586 = LINE ( 'NONE', #3501, #13576 ) ;
#2587 = ORIENTED_EDGE ( 'NONE', *, *, #5028, .F. ) ;
#2588 = EDGE_CURVE ( 'NONE', #6001, #11537, #12107, .T. ) ;
#2589 = ADVANCED_FACE ( 'NONE', ( #4975 ), #1355, .F. ) ;
#2590 = DIRECTION ( 'NONE',  ( -1.000000000000000000, -0.000000000000000000, -0.000000000000000000 ) ) ;
#2591 = DIRECTION ( 'NONE',  ( 0.9999002670844990837, 1.110054405283695815E-35, -0.01412288512831213171 ) ) ;
#2592 = ORIENTED_EDGE ( 'NONE', *, *, #8020, .F. ) ;
#2593 = ADVANCED_FACE ( 'NONE', ( #11854 ), #9780, .F. ) ;
#2594 = DIRECTION ( 'NONE',  ( 1.000000000000000000, 0.000000000000000000, 0.000000000000000000 ) ) ;
#2595 = CARTESIAN_POINT ( 'NONE',  ( 0.7058998964907862161, -0.05999999999999994227, 0.4900296624789436950 ) ) ;
#2596 = AXIS2_PLACEMENT_3D ( 'NONE', #2608, #1140, #5830 ) ;
#2597 = CARTESIAN_POINT ( 'NONE',  ( 0.9176380235743000213, 0.1749999999999999889, -0.1164708448095589793 ) ) ;
#2598 = PLANE ( 'NONE',  #1298 ) ;
#2599 = CONICAL_SURFACE ( 'NONE', #7470, 2.967999999999998639, 0.7853981633974482790 ) ;
#2600 = EDGE_CURVE ( 'NONE', #2516, #4201, #5523, .T. ) ;
#2601 = CARTESIAN_POINT ( 'NONE',  ( 8.575402687747825325, 0.8724108505555134840, 0.3686609533459700438 ) ) ;
#2602 = CARTESIAN_POINT ( 'NONE',  ( 0.8374477884936026850, -0.4460803254964525455, -0.4171268816085695885 ) ) ;
#2603 = CARTESIAN_POINT ( 'NONE',  ( 0.06299999999999994493, 3.654346048655701274E-16, 2.967999999999998639 ) ) ;
#2604 = CARTESIAN_POINT ( 'NONE',  ( 4.572381542873881877, 1.717371224058993340, -0.4020716753058218296 ) ) ;
#2605 = TOROIDAL_SURFACE ( 'NONE', #4072, 0.8653656741516848605, 0.05999999999999999778 ) ;
#2606 = VERTEX_POINT ( 'NONE', #5125 ) ;
#2607 = CARTESIAN_POINT ( 'NONE',  ( 0.6601485485260571995, -0.3723516483516483011, 0.5137583810202324131 ) ) ;
#2609 = ORIENTED_EDGE ( 'NONE', *, *, #10633, .F. ) ;
#2608 = CARTESIAN_POINT ( 'NONE',  ( 0.8999999999999999112, -0.6429999999999999050, -0.3750000000000000555 ) ) ;
#2610 = EDGE_LOOP ( 'NONE', ( #10486, #5324 ) ) ;
#2611 = EDGE_CURVE ( 'NONE', #2748, #3130, #4056, .T. ) ;
#2612 = CARTESIAN_POINT ( 'NONE',  ( 3.875000000000000000, 1.112678268764263789, 0.4849999999999995981 ) ) ;
#2613 = FACE_OUTER_BOUND ( 'NONE', #509, .T. ) ;
#2614 = ORIENTED_EDGE ( 'NONE', *, *, #1520, .T. ) ;
#2615 = CARTESIAN_POINT ( 'NONE',  ( 2.034127966794863518, -0.2372991579513219207, 0.4117015842447220852 ) ) ;
#2616 = VECTOR ( 'NONE', #3332, 39.37007874015748143 ) ;
#2617 = DIRECTION ( 'NONE',  ( -1.000000000000000000, -0.000000000000000000, -0.000000000000000000 ) ) ;
#2618 = CARTESIAN_POINT ( 'NONE',  ( -0.4425000000000007261, 0.2159999999999999420, -0.8499999999999999778 ) ) ;
#2619 = ADVANCED_FACE ( 'NONE', ( #4825 ), #2576, .T. ) ;
#2620 = ORIENTED_EDGE ( 'NONE', *, *, #2538, .F. ) ;
#2621 = FACE_OUTER_BOUND ( 'NONE', #3128, .T. ) ;
#2622 = DIRECTION ( 'NONE',  ( -1.655665450705613915E-16, 0.000000000000000000, -1.000000000000000000 ) ) ;
#2623 = DIRECTION ( 'NONE',  ( 0.000000000000000000, 0.000000000000000000, 1.000000000000000000 ) ) ;
#2624 = ORIENTED_EDGE ( 'NONE', *, *, #12278, .T. ) ;
#2625 = EDGE_CURVE ( 'NONE', #7690, #1866, #13430, .T. ) ;
#2626 = DIRECTION ( 'NONE',  ( 0.000000000000000000, 0.000000000000000000, 1.000000000000000000 ) ) ;
#2627 = ORIENTED_EDGE ( 'NONE', *, *, #4803, .T. ) ;
#2628 = VECTOR ( 'NONE', #93, 39.37007874015748143 ) ;
#2629 = CARTESIAN_POINT ( 'NONE',  ( -0.2249147617188618498, 1.559103846021574258, 0.3723417112826993836 ) ) ;
#2630 = EDGE_LOOP ( 'NONE', ( #9539, #10916, #3560, #6578, #13082, #6957, #8243 ) ) ;
#2631 = CARTESIAN_POINT ( 'NONE',  ( 2.282850251811050946, 0.09542856769866185640, -0.4677563523755502994 ) ) ;
#2632 = VECTOR ( 'NONE', #339, 39.37007874015748143 ) ;
#2633 = CYLINDRICAL_SURFACE ( 'NONE', #4350, 0.03999999999999998002 ) ;
#2634 = CARTESIAN_POINT ( 'NONE',  ( 3.426491571325181340, -2.360000000000016751, -0.9799999999999431388 ) ) ;
#2635 = CARTESIAN_POINT ( 'NONE',  ( 2.774999999999999911, -1.575000000000027489, -2.359999999999989218 ) ) ;
#2636 = ADVANCED_FACE ( 'NONE', ( #8083 ), #11146, .F. ) ;
#2637 = CIRCLE ( 'NONE', #11179, 0.03999999999999998002 ) ;
#2638 = ADVANCED_FACE ( 'NONE', ( #10087 ), #10016, .T. ) ;
#2639 = VERTEX_POINT ( 'NONE', #12219 ) ;
#2640 = ORIENTED_EDGE ( 'NONE', *, *, #3537, .T. ) ;
#2641 = AXIS2_PLACEMENT_3D ( 'NONE', #6563, #11221, #718 ) ;
#2642 = VERTEX_POINT ( 'NONE', #14670 ) ;
#2643 = LINE ( 'NONE', #3870, #5524 ) ;
#2644 = DIRECTION ( 'NONE',  ( 0.000000000000000000, -1.000000000000000000, 0.000000000000000000 ) ) ;
#2645 = PLANE ( 'NONE',  #11277 ) ;
#2646 = CARTESIAN_POINT ( 'NONE',  ( 0.6500000000000001332, -1.679378605318048390, 1.679378605318054163 ) ) ;
#2647 = VECTOR ( 'NONE', #9467, 39.37007874015748143 ) ;
#2648 = CARTESIAN_POINT ( 'NONE',  ( 3.851988768209213987, 1.889494746496508393, -0.4996036056591527941 ) ) ;
#2649 = AXIS2_PLACEMENT_3D ( 'NONE', #14520, #6365, #11083 ) ;
#2650 = APPLICATION_CONTEXT ( 'automotive_design' ) ;
#2651 = CARTESIAN_POINT ( 'NONE',  ( 1.748545107151218803, 0.1138129195078394773, 0.4149214987681951738 ) ) ;
#2652 = DIRECTION ( 'NONE',  ( -1.000000000000000000, 0.000000000000000000, 0.000000000000000000 ) ) ;
#2653 = VECTOR ( 'NONE', #10801, 39.37007874015748854 ) ;
#2654 = CIRCLE ( 'NONE', #11200, 1.875500000000000167 ) ;
#2655 = CONICAL_SURFACE ( 'NONE', #11707, 1.875000000000000000, 0.7853981633974482790 ) ;
#2656 = EDGE_CURVE ( 'NONE', #3185, #11461, #4197, .T. ) ;
#2657 = AXIS2_PLACEMENT_3D ( 'NONE', #9521, #4696, #1154 ) ;
#2658 = ORIENTED_EDGE ( 'NONE', *, *, #14455, .F. ) ;
#2660 = ORIENTED_EDGE ( 'NONE', *, *, #14939, .F. ) ;
#2659 = CYLINDRICAL_SURFACE ( 'NONE', #7418, 0.2625000000000000111 ) ;
#2661 = CIRCLE ( 'NONE', #7789, 0.05999999999999996309 ) ;
#2662 = ORIENTED_EDGE ( 'NONE', *, *, #11568, .T. ) ;
#2663 = DIRECTION ( 'NONE',  ( 0.000000000000000000, -1.000000000000000000, 0.000000000000000000 ) ) ;
#2664 = ORIENTED_EDGE ( 'NONE', *, *, #8629, .F. ) ;
#2665 = DIRECTION ( 'NONE',  ( 0.000000000000000000, -0.7071067811865452413, -0.7071067811865496822 ) ) ;
#2666 = PRODUCT_CONTEXT ( 'NONE', #2650, 'mechanical' ) ;
#2667 = CARTESIAN_POINT ( 'NONE',  ( 2.381437798646956594, 0.6472152511680805409, 0.4058409478271199355 ) ) ;
#2668 = ORIENTED_EDGE ( 'NONE', *, *, #7606, .F. ) ;
#2669 =( BOUNDED_SURFACE ( )  B_SPLINE_SURFACE ( 3, 2, ( 
 ( #2737, #8486, #14352 ),
 ( #485, #12210, #1792 ),
 ( #1718, #11138, #11061 ),
 ( #14662, #12063, #14578 ),
 ( #556, #1570, #4106 ),
 ( #8779, #6261, #637 ),
 ( #7620, #5334, #13127 ),
 ( #2667, #7340, #10924 ),
 ( #11992, #10228, #11293 ),
 ( #10301, #4417, #6787 ) ),
 .UNSPECIFIED., .F., .F., .F. ) 
 B_SPLINE_SURFACE_WITH_KNOTS ( ( 4, 2, 2, 2, 4 ),
 ( 3, 3 ),
 ( 1.570796326794896558, 1.767145867644259294, 1.963495408493621808, 2.159844949342984322, 2.356194490192347057 ),
 ( 0.000000000000000000, 1.000000000000000000 ),
 .UNSPECIFIED. ) 
 GEOMETRIC_REPRESENTATION_ITEM ( )  RATIONAL_B_SPLINE_SURFACE ( (
 ( 1.000000000000000000, 0.7071067811865475727, 1.000000000000000000),
 ( 1.000000000000000000, 0.7067799747771658092, 1.000000000000000000),
 ( 1.000000000000000000, 0.7064529522744581458, 1.000000000000000000),
 ( 1.000000000000000000, 0.7058110186548579579, 1.000000000000000000),
 ( 1.000000000000000000, 0.7054961263481117628, 1.000000000000000000),
 ( 1.000000000000000000, 0.7048906332637320249, 1.000000000000000000),
 ( 1.000000000000000000, 0.7046000480541857458, 1.000000000000000000),
 ( 1.000000000000000000, 0.7040544485618952519, 1.000000000000000000),
 ( 1.000000000000000000, 0.7037994241806829754, 1.000000000000000000),
 ( 1.000000000000000000, 0.7035672008258530008, 1.000000000000000000) ) ) 
 REPRESENTATION_ITEM ( '' )  SURFACE ( )  );
#2670 = CIRCLE ( 'NONE', #15119, 0.8000000000000000444 ) ;
#2671 = DIRECTION ( 'NONE',  ( 0.000000000000000000, 0.000000000000000000, 1.000000000000000000 ) ) ;
#2672 = FACE_OUTER_BOUND ( 'NONE', #1523, .T. ) ;
#2673 = CARTESIAN_POINT ( 'NONE',  ( 6.826491571325181695, -1.679378605318047946, -1.679378605318053497 ) ) ;
#2674 = PLANE ( 'NONE',  #5719 ) ;
#2675 = AXIS2_PLACEMENT_3D ( 'NONE', #14893, #5876, #11603 ) ;
#2676 = CARTESIAN_POINT ( 'NONE',  ( 2.774999999999999911, -1.574999999999984190, 1.575000000000033040 ) ) ;
#2677 = CARTESIAN_POINT ( 'NONE',  ( 0.8725078605757294881, -0.4668629105576758143, -0.4450936002735125241 ) ) ;
#2678 = CARTESIAN_POINT ( 'NONE',  ( 6.176491571325181340, -1.679378605318047946, -1.679378605318053497 ) ) ;
#2679 = CARTESIAN_POINT ( 'NONE',  ( 3.550764771811983245, 1.993778310833772105, 0.6763632542489218524 ) ) ;
#2680 = CARTESIAN_POINT ( 'NONE',  ( 2.774999999999999911, -0.9799999999999436939, 3.360000000000016751 ) ) ;
#2681 = VERTEX_POINT ( 'NONE', #1881 ) ;
#2682 = CARTESIAN_POINT ( 'NONE',  ( 8.474190026735612946, 1.056999999999999940, -0.3203020658980470503 ) ) ;
#2684 = EDGE_LOOP ( 'NONE', ( #2658, #13898, #14726, #8637 ) ) ;
#2683 = FACE_BOUND ( 'NONE', #11984, .T. ) ;
#2685 = ORIENTED_EDGE ( 'NONE', *, *, #12432, .T. ) ;
#2686 = AXIS2_PLACEMENT_3D ( 'NONE', #14325, #8531, #3860 ) ;
#2687 = CARTESIAN_POINT ( 'NONE',  ( 0.8083085967350902568, -0.4844395604395603239, 0.000000000000000000 ) ) ;
#2688 =( NAMED_UNIT ( * ) PLANE_ANGLE_UNIT ( ) SI_UNIT ( $, .RADIAN. ) );
#2689 = CARTESIAN_POINT ( 'NONE',  ( 0.1164708448095412852, 0.1749999999999999889, -0.9176380235743023528 ) ) ;
#2690 = VERTEX_POINT ( 'NONE', #10365 ) ;
#2691 = DIRECTION ( 'NONE',  ( 0.9999002670844989726, -2.602203049398213494E-17, -0.01412288512831212997 ) ) ;
#2692 = CARTESIAN_POINT ( 'NONE',  ( 0.6570985677785575740, -0.05542231959448562506, 0.5130299739594185171 ) ) ;
#2693 = ADVANCED_FACE ( 'NONE', ( #723 ), #9443, .F. ) ;
#2694 = FACE_OUTER_BOUND ( 'NONE', #10464, .T. ) ;
#2695 = VECTOR ( 'NONE', #417, 39.37007874015748143 ) ;
#2696 = ADVANCED_FACE ( 'NONE', ( #11514 ), #3038, .F. ) ;
#2697 = EDGE_LOOP ( 'NONE', ( #5764, #4410, #8464, #10131 ) ) ;
#2698 = EDGE_CURVE ( 'NONE', #1992, #11318, #4553, .T. ) ;
#2699 = CARTESIAN_POINT ( 'NONE',  ( 1.003096136995459631, -0.4429976034824900655, -0.4258273028168327867 ) ) ;
#2700 = DIRECTION ( 'NONE',  ( 0.7071067811865429098, 0.000000000000000000, -0.7071067811865521247 ) ) ;
#2701 = DIRECTION ( 'NONE',  ( 0.000000000000000000, 0.000000000000000000, -1.000000000000000000 ) ) ;
#2702 = ORIENTED_EDGE ( 'NONE', *, *, #5994, .T. ) ;
#2703 = CARTESIAN_POINT ( 'NONE',  ( 2.774999999999999911, -3.360000000000000320, 0.9799999999999999822 ) ) ;
#2704 = DIRECTION ( 'NONE',  ( 0.7071067811865474617, 0.000000000000000000, -0.7071067811865474617 ) ) ;
#2705 = ORIENTED_EDGE ( 'NONE', *, *, #1557, .F. ) ;
#2706 = EDGE_CURVE ( 'NONE', #2583, #11671, #5278, .T. ) ;
#2707 = CARTESIAN_POINT ( 'NONE',  ( 0.7038889044926298633, -0.05564817238903751323, 0.4900580663207255716 ) ) ;
#2708 = VERTEX_POINT ( 'NONE', #1724 ) ;
#2709 = DIRECTION ( 'NONE',  ( -1.000000000000000000, -0.000000000000000000, -0.000000000000000000 ) ) ;
#2710 = CARTESIAN_POINT ( 'NONE',  ( 3.874999999999999556, 3.105999999999998984, 1.509999999999999787 ) ) ;
#2711 = DIRECTION ( 'NONE',  ( 0.000000000000000000, 0.000000000000000000, -1.000000000000000000 ) ) ;
#2712 = LINE ( 'NONE', #2854, #12650 ) ;
#2713 = FACE_OUTER_BOUND ( 'NONE', #3435, .T. ) ;
#2714 = VECTOR ( 'NONE', #1879, 39.37007874015748143 ) ;
#2715 = ORIENTED_EDGE ( 'NONE', *, *, #7536, .F. ) ;
#2716 = ORIENTED_EDGE ( 'NONE', *, *, #9923, .F. ) ;
#2717 = ORIENTED_EDGE ( 'NONE', *, *, #9399, .F. ) ;
#2718 = ADVANCED_FACE ( 'NONE', ( #6347 ), #493, .F. ) ;
#2719 = DIRECTION ( 'NONE',  ( -0.7071067811865414665, 8.659560562355006814E-17, -0.7071067811865534569 ) ) ;
#2720 = CARTESIAN_POINT ( 'NONE',  ( -0.3725000000000000533, -0.6590000000000000302, 0.4424999999999981726 ) ) ;
#2721 = ADVANCED_FACE ( 'NONE', ( #14584 ), #11374, .F. ) ;
#2722 = CARTESIAN_POINT ( 'NONE',  ( 1.000048944713735732, -0.4428998280398802612, -0.4293350073753851581 ) ) ;
#2723 = CARTESIAN_POINT ( 'NONE',  ( 3.426491571325181340, -1.679378605318059048, -1.416878605318056872 ) ) ;
#2724 = AXIS2_PLACEMENT_3D ( 'NONE', #10655, #73, #3620 ) ;
#2725 = CARTESIAN_POINT ( 'NONE',  ( 6.787121492585022509, 0.000000000000000000, 0.000000000000000000 ) ) ;
#2726 = EDGE_CURVE ( 'NONE', #9791, #628, #3712, .T. ) ;
#2727 = CARTESIAN_POINT ( 'NONE',  ( 2.774999999999999911, 0.9799999999999438050, -2.360000000000016307 ) ) ;
#2728 = CARTESIAN_POINT ( 'NONE',  ( 2.156999999999998696, -1.679378605318059048, -1.941878605318027251 ) ) ;
#2729 = DIRECTION ( 'NONE',  ( 0.000000000000000000, 0.000000000000000000, -1.000000000000000000 ) ) ;
#2730 = AXIS2_PLACEMENT_3D ( 'NONE', #2864, #1555, #1484 ) ;
#2731 = ORIENTED_EDGE ( 'NONE', *, *, #10258, .T. ) ;
#2732 = ORIENTED_EDGE ( 'NONE', *, *, #6388, .F. ) ;
#2733 = ORIENTED_EDGE ( 'NONE', *, *, #10286, .F. ) ;
#2734 = DIRECTION ( 'NONE',  ( -0.7071067811865376918, 0.000000000000000000, 0.7071067811865573427 ) ) ;
#2735 = DIRECTION ( 'NONE',  ( 1.000000000000000000, 0.000000000000000000, 0.000000000000000000 ) ) ;
#2736 = CARTESIAN_POINT ( 'NONE',  ( 4.329878488001781101, 0.9782040126189885942, -0.2082197225034957411 ) ) ;
#2737 = CARTESIAN_POINT ( 'NONE',  ( 3.601417382415921686, 1.056999999999999718, 0.3891265382754439117 ) ) ;
#2738 = ORIENTED_EDGE ( 'NONE', *, *, #8998, .F. ) ;
#2739 = CARTESIAN_POINT ( 'NONE',  ( 1.000000000000000222, -0.3829999999999998961, 0.4258697216429003785 ) ) ;
#2740 = CARTESIAN_POINT ( 'NONE',  ( 0.000000000000000000, 0.000000000000000000, 0.000000000000000000 ) ) ;
#2741 = EDGE_CURVE ( 'NONE', #1223, #7612, #12351, .T. ) ;
#2742 = LINE ( 'NONE', #1278, #11744 ) ;
#2743 = DIRECTION ( 'NONE',  ( -0.000000000000000000, -1.000000000000000000, 0.000000000000000000 ) ) ;
#2744 = DIRECTION ( 'NONE',  ( -0.000000000000000000, -1.000000000000000000, -0.000000000000000000 ) ) ;
#2745 = CARTESIAN_POINT ( 'NONE',  ( 0.4124999999999997558, 0.1859999999999983611, -0.3725000000000000533 ) ) ;
#2746 = CARTESIAN_POINT ( 'NONE',  ( 3.772736115549563340, 1.833816802295039849, 0.7431948924224894837 ) ) ;
#2747 = DIRECTION ( 'NONE',  ( 0.000000000000000000, 0.000000000000000000, 1.000000000000000000 ) ) ;
#2748 = VERTEX_POINT ( 'NONE', #4786 ) ;
#2749 = CARTESIAN_POINT ( 'NONE',  ( 2.124999999999999556, -0.9799999999999436939, 2.360000000000016307 ) ) ;
#2751 = ORIENTED_EDGE ( 'NONE', *, *, #233, .T. ) ;
#2750 = CARTESIAN_POINT ( 'NONE',  ( 0.6179999999999962190, -1.679378605318048390, 1.679378605318054163 ) ) ;
#2752 = ORIENTED_EDGE ( 'NONE', *, *, #14636, .F. ) ;
#2753 = CARTESIAN_POINT ( 'NONE',  ( 3.873439288382781065, 2.750000000000000000, 6.065921084684207584E-32 ) ) ;
#2754 = CARTESIAN_POINT ( 'NONE',  ( 2.980731298636167370, 3.567999999999999616, 0.3249191361593796179 ) ) ;
#2755 = ORIENTED_EDGE ( 'NONE', *, *, #6528, .T. ) ;
#2756 = CONICAL_SURFACE ( 'NONE', #992, 0.2945000000000006501, 0.7853981633974503884 ) ;
#2757 = DIRECTION ( 'NONE',  ( 0.000000000000000000, 0.000000000000000000, -1.000000000000000000 ) ) ;
#2758 = AXIS2_PLACEMENT_3D ( 'NONE', #3900, #13061, #3826 ) ;
#2759 = ADVANCED_FACE ( 'NONE', ( #3642 ), #2835, .T. ) ;
#2760 = TOROIDAL_SURFACE ( 'NONE', #4473, 0.1150000000000000050, 0.04000000000000000083 ) ;
#2761 = CARTESIAN_POINT ( 'NONE',  ( 0.6601485485260575325, -0.07064835164835217562, 0.5137583810202324131 ) ) ;
#2762 = DIRECTION ( 'NONE',  ( 1.000000000000000000, 0.000000000000000000, 0.000000000000000000 ) ) ;
#2763 = VERTEX_POINT ( 'NONE', #10591 ) ;
#2764 = LINE ( 'NONE', #7434, #9505 ) ;
#2765 = VECTOR ( 'NONE', #14269, 39.37007874015748143 ) ;
#2766 = CARTESIAN_POINT ( 'NONE',  ( 2.774999999999999911, 0.000000000000000000, 0.000000000000000000 ) ) ;
#2767 = CARTESIAN_POINT ( 'NONE',  ( 2.743000000000000327, 1.679378605318042395, -1.941878605318058115 ) ) ;
#2768 = EDGE_LOOP ( 'NONE', ( #1446, #7479, #6384 ) ) ;
#2769 = FACE_OUTER_BOUND ( 'NONE', #4960, .T. ) ;
#2770 = ORIENTED_EDGE ( 'NONE', *, *, #12262, .T. ) ;
#2771 = FACE_OUTER_BOUND ( 'NONE', #6150, .T. ) ;
#2772 = ORIENTED_EDGE ( 'NONE', *, *, #8012, .T. ) ;
#2773 = EDGE_CURVE ( 'NONE', #3609, #5110, #5774, .T. ) ;
#2774 =( CONVERSION_BASED_UNIT ( 'INCH', #13234 ) LENGTH_UNIT ( ) NAMED_UNIT ( #12236 ) );
#2775 = ADVANCED_FACE ( 'NONE', ( #1091 ), #15101, .F. ) ;
#2776 = ADVANCED_FACE ( 'NONE', ( #13023 ), #8322, .F. ) ;
#2777 = AXIS2_PLACEMENT_3D ( 'NONE', #8442, #12313, #5369 ) ;
#2778 = CARTESIAN_POINT ( 'NONE',  ( 2.806999999999999940, -1.679378605318059048, -1.941878605318027251 ) ) ;
#2779 = VECTOR ( 'NONE', #3299, 39.37007874015748143 ) ;
#2780 = CYLINDRICAL_SURFACE ( 'NONE', #11916, 0.05999999999999983818 ) ;
#2781 = CLOSED_SHELL ( 'NONE', ( #2759, #10821, #1746, #795, #9814, #5799, #13934, #5060 ) ) ;
#2782 = DIRECTION ( 'NONE',  ( -0.000000000000000000, -1.000000000000000000, -0.000000000000000000 ) ) ;
#2783 = ADVANCED_FACE ( 'NONE', ( #6088 ), #3478, .F. ) ;
#2784 = CARTESIAN_POINT ( 'NONE',  ( 3.444319122601930972E-17, 1.249999999999999778, 0.2812500000000000555 ) ) ;
#2785 = LINE ( 'NONE', #1767, #5454 ) ;
#2786 = CIRCLE ( 'NONE', #5229, 1.350000000000000089 ) ;
#2787 = ORIENTED_EDGE ( 'NONE', *, *, #13414, .T. ) ;
#2788 = ORIENTED_EDGE ( 'NONE', *, *, #13561, .T. ) ;
#2789 = ORIENTED_EDGE ( 'NONE', *, *, #13488, .T. ) ;
#2790 = CARTESIAN_POINT ( 'NONE',  ( 8.707077114626844860, 0.8770090228646982844, -0.3011897810130372832 ) ) ;
#2791 = DIRECTION ( 'NONE',  ( 0.000000000000000000, -4.591341165822158293E-16, 1.000000000000000000 ) ) ;
#2792 = DIRECTION ( 'NONE',  ( 1.000000000000000000, 0.000000000000000000, 0.000000000000000000 ) ) ;
#2793 = DIRECTION ( 'NONE',  ( 0.000000000000000000, 0.000000000000000000, 1.000000000000000000 ) ) ;
#2794 = CARTESIAN_POINT ( 'NONE',  ( 3.426491571325181340, -0.9799999999999436939, 2.360000000000016307 ) ) ;
#2795 = CARTESIAN_POINT ( 'NONE',  ( 4.146569453972532848, 1.792765056676476121, 0.6998195859356590720 ) ) ;
#2796 = VECTOR ( 'NONE', #8805, 39.37007874015748143 ) ;
#2797 = EDGE_CURVE ( 'NONE', #13738, #4021, #14499, .T. ) ;
#2798 = ADVANCED_FACE ( 'NONE', ( #2486 ), #8157, .F. ) ;
#2799 = ORIENTED_EDGE ( 'NONE', *, *, #5375, .T. ) ;
#2800 = ORIENTED_EDGE ( 'NONE', *, *, #8594, .F. ) ;
#2801 = EDGE_CURVE ( 'NONE', #1793, #1160, #859, .T. ) ;
#2802 = VECTOR ( 'NONE', #11427, 39.37007874015748143 ) ;
#2803 = EDGE_LOOP ( 'NONE', ( #858, #3536 ) ) ;
#2804 = CARTESIAN_POINT ( 'NONE',  ( 0.000000000000000000, 0.000000000000000000, 1.125000000000000888 ) ) ;
#2805 = AXIS2_PLACEMENT_3D ( 'NONE', #4001, #5086, #8670 ) ;
#2806 = VECTOR ( 'NONE', #2617, 39.37007874015748143 ) ;
#2807 = DIRECTION ( 'NONE',  ( -0.000000000000000000, -1.000000000000000000, -0.000000000000000000 ) ) ;
#2808 = DIRECTION ( 'NONE',  ( 0.000000000000000000, 1.000000000000000000, -0.000000000000000000 ) ) ;
#2809 = SHAPE_DEFINITION_REPRESENTATION ( #7272, #1600 ) ;
#2810 = DIRECTION ( 'NONE',  ( 0.000000000000000000, 0.000000000000000000, -1.000000000000000000 ) ) ;
#2811 = ORIENTED_EDGE ( 'NONE', *, *, #9367, .F. ) ;
#2812 = DIRECTION ( 'NONE',  ( -0.000000000000000000, -1.000000000000000000, -0.000000000000000000 ) ) ;
#2813 = DIRECTION ( 'NONE',  ( -0.000000000000000000, -0.000000000000000000, 1.000000000000000000 ) ) ;
#2814 = DIRECTION ( 'NONE',  ( -0.000000000000000000, -1.000000000000000000, 0.000000000000000000 ) ) ;
#2815 = AXIS2_PLACEMENT_3D ( 'NONE', #2039, #10473, #10622 ) ;
#2816 = DIRECTION ( 'NONE',  ( 1.000000000000000000, 0.000000000000000000, 0.000000000000000000 ) ) ;
#2817 = AXIS2_PLACEMENT_3D ( 'NONE', #2245, #11582, #8233 ) ;
#2818 = CIRCLE ( 'NONE', #347, 1.749999999999999556 ) ;
#2819 = CARTESIAN_POINT ( 'NONE',  ( -5.764454660286586870E-18, 0.1956296296296295978, 0.000000000000000000 ) ) ;
#2820 = CARTESIAN_POINT ( 'NONE',  ( 3.411537114321682385, 2.070878521370026704, 0.5884327097963867326 ) ) ;
#2821 = DIRECTION ( 'NONE',  ( -0.7071067811865425767, 0.000000000000000000, 0.7071067811865523467 ) ) ;
#2822 = EDGE_CURVE ( 'NONE', #10976, #3309, #11817, .T. ) ;
#2823 = EDGE_CURVE ( 'NONE', #12211, #5232, #8236, .T. ) ;
#2824 = ORIENTED_EDGE ( 'NONE', *, *, #7030, .F. ) ;
#2825 = DIRECTION ( 'NONE',  ( 0.000000000000000000, 0.000000000000000000, -1.000000000000000000 ) ) ;
#2827 = EDGE_LOOP ( 'NONE', ( #654, #1518, #9071, #5555 ) ) ;
#2826 = CARTESIAN_POINT ( 'NONE',  ( 3.394491571325183088, 1.679378605318059048, 1.679378605318041506 ) ) ;
#2828 = VERTEX_POINT ( 'NONE', #17 ) ;
#2829 = DIRECTION ( 'NONE',  ( 0.000000000000000000, -0.000000000000000000, 1.000000000000000000 ) ) ;
#2830 = CONICAL_SURFACE ( 'NONE', #2334, 0.3750000000000004996, 0.7853981633974503884 ) ;
#2831 = CARTESIAN_POINT ( 'NONE',  ( 2.774999999999999911, 0.000000000000000000, 0.000000000000000000 ) ) ;
#2832 = ORIENTED_EDGE ( 'NONE', *, *, #6418, .T. ) ;
#2833 = CARTESIAN_POINT ( 'NONE',  ( 2.774999999999999911, -2.399999999999999911, 0.7000000000000007327 ) ) ;
#2834 = DIRECTION ( 'NONE',  ( 0.000000000000000000, 9.182682331643740718E-16, -1.000000000000000000 ) ) ;
#2835 = TOROIDAL_SURFACE ( 'NONE', #7247, 0.5849999999999996314, 0.1000000000000000056 ) ;
#2836 = AXIS2_PLACEMENT_3D ( 'NONE', #11592, #1097, #3484 ) ;
#2837 = CARTESIAN_POINT ( 'NONE',  ( 0.7050899422473002609, -0.02184511171346635930, 0.4765263839844876004 ) ) ;
#2838 = DIRECTION ( 'NONE',  ( -1.000000000000000000, -0.000000000000000000, -0.000000000000000000 ) ) ;
#2839 = VERTEX_POINT ( 'NONE', #2409 ) ;
#2840 = LINE ( 'NONE', #10877, #2168 ) ;
#2841 = CARTESIAN_POINT ( 'NONE',  ( 8.474190026735612946, 0.9289129992088663856, -0.3203020658980469948 ) ) ;
#2842 = DIRECTION ( 'NONE',  ( 0.000000000000000000, 0.000000000000000000, -1.000000000000000000 ) ) ;
#2843 = AXIS2_PLACEMENT_3D ( 'NONE', #7989, #14944, #6851 ) ;
#2844 = VERTEX_POINT ( 'NONE', #10672 ) ;
#2845 = DIRECTION ( 'NONE',  ( -1.000000000000000000, -0.000000000000000000, -0.000000000000000000 ) ) ;
#2846 = ORIENTED_EDGE ( 'NONE', *, *, #14082, .T. ) ;
#2847 = CARTESIAN_POINT ( 'NONE',  ( 0.7513246802501660770, 0.000000000000000000, 0.4293820849162031661 ) ) ;
#2848 = ORIENTED_EDGE ( 'NONE', *, *, #5411, .T. ) ;
#2849 = CYLINDRICAL_SURFACE ( 'NONE', #12927, 0.7849999999999958122 ) ;
#2850 = CIRCLE ( 'NONE', #6275, 0.4070000000000025264 ) ;
#2851 = CARTESIAN_POINT ( 'NONE',  ( 0.8999999999999998002, 0.1549999999999996103, -0.4650000000000000244 ) ) ;
#2852 = CARTESIAN_POINT ( 'NONE',  ( 0.8321316902697376561, -0.4837345936509453437, -0.3428764643457666850 ) ) ;
#2853 = AXIS2_PLACEMENT_3D ( 'NONE', #13265, #2807, #2877 ) ;
#2854 = CARTESIAN_POINT ( 'NONE',  ( 6.176491571325181340, 1.679378605318035733, -1.272378605318063016 ) ) ;
#2855 = CARTESIAN_POINT ( 'NONE',  ( 3.426491571325181340, 1.679378605318042395, -1.679378605318058604 ) ) ;
#2856 = EDGE_CURVE ( 'NONE', #6694, #5312, #10178, .T. ) ;
#2857 = DIRECTION ( 'NONE',  ( 0.000000000000000000, 0.000000000000000000, -1.000000000000000000 ) ) ;
#2858 = ORIENTED_EDGE ( 'NONE', *, *, #1785, .F. ) ;
#2859 = VERTEX_POINT ( 'NONE', #2562 ) ;
#2860 = ORIENTED_EDGE ( 'NONE', *, *, #9184, .T. ) ;
#2861 = CARTESIAN_POINT ( 'NONE',  ( 8.635695252271261779, 0.8745163133035791514, -0.2783269381325276237 ) ) ;
#2862 = CARTESIAN_POINT ( 'NONE',  ( 2.774999999999999911, 1.679378605318042395, -1.679378605318058604 ) ) ;
#2863 = AXIS2_PLACEMENT_3D ( 'NONE', #14207, #5963, #267 ) ;
#2864 = CARTESIAN_POINT ( 'NONE',  ( 3.875000000000000000, 3.137999999999999901, 0.000000000000000000 ) ) ;
#2865 = EDGE_CURVE ( 'NONE', #6548, #1865, #13545, .T. ) ;
#2866 = CARTESIAN_POINT ( 'NONE',  ( 3.394491571325183088, 1.679378605318059048, 1.416878605318041551 ) ) ;
#2867 = PRODUCT_DEFINITION_SHAPE ( 'NONE', 'NONE',  #4715 ) ;
#2868 = CARTESIAN_POINT ( 'NONE',  ( 3.426491571325180452, 2.038249570078020767, -0.6032545795923431875 ) ) ;
#2869 = CARTESIAN_POINT ( 'NONE',  ( 2.124999999999999556, 0.000000000000000000, 0.000000000000000000 ) ) ;
#2870 = EDGE_CURVE ( 'NONE', #11436, #11127, #242, .T. ) ;
#2871 = CIRCLE ( 'NONE', #14851, 1.580000000000000071 ) ;
#2872 = EDGE_CURVE ( 'NONE', #10222, #4965, #1397, .T. ) ;
#2873 = ORIENTED_EDGE ( 'NONE', *, *, #14209, .T. ) ;
#2874 = VERTEX_POINT ( 'NONE', #306 ) ;
#2875 = ORIENTED_EDGE ( 'NONE', *, *, #5133, .F. ) ;
#2876 = CARTESIAN_POINT ( 'NONE',  ( 1.000000000000000000, -0.4429999999999998939, 0.5000000000000000000 ) ) ;
#2877 = DIRECTION ( 'NONE',  ( 0.000000000000000000, 0.000000000000000000, -1.000000000000000000 ) ) ;
#2879 = VECTOR ( 'NONE', #685, 39.37007874015748854 ) ;
#2878 = CARTESIAN_POINT ( 'NONE',  ( 4.251234628174230146, 0.9439865100702572454, 0.3308754778004969754 ) ) ;
#2880 = EDGE_CURVE ( 'NONE', #3585, #7387, #1475, .T. ) ;
#2881 = CARTESIAN_POINT ( 'NONE',  ( 0.7936328852534487721, 0.1749999999999999889, -0.1007315414569158740 ) ) ;
#2882 = ORIENTED_EDGE ( 'NONE', *, *, #11350, .T. ) ;
#2883 = LINE ( 'NONE', #13202, #1392 ) ;
#2884 = CARTESIAN_POINT ( 'NONE',  ( 2.774999999999999911, -1.679378605318041950, 1.384878605318060174 ) ) ;
#2885 = VECTOR ( 'NONE', #6652, 39.37007874015748854 ) ;
#2886 = EDGE_CURVE ( 'NONE', #8576, #9649, #13059, .T. ) ;
#2887 = CYLINDRICAL_SURFACE ( 'NONE', #13355, 2.500000000000000000 ) ;
#2888 = AXIS2_PLACEMENT_3D ( 'NONE', #6380, #531, #4077 ) ;
#2889 = AXIS2_PLACEMENT_3D ( 'NONE', #9496, #11783, #2371 ) ;
#2890 = AXIS2_PLACEMENT_3D ( 'NONE', #14482, #8681, #13011 ) ;
#2891 = CARTESIAN_POINT ( 'NONE',  ( 8.729039508763705157, 0.8777759665679295553, 0.1953148678277666916 ) ) ;
#2892 = CIRCLE ( 'NONE', #7534, 0.1899999999999996136 ) ;
#2893 = CARTESIAN_POINT ( 'NONE',  ( 0.9947690811584967152, -0.4425817642695075715, -0.4349075309858640992 ) ) ;
#2894 = CARTESIAN_POINT ( 'NONE',  ( 3.464768837743798180, 2.040166567261363806, 0.6277031159343403610 ) ) ;
#2896 = EDGE_LOOP ( 'NONE', ( #8452, #6111, #9278, #9671 ) ) ;
#2895 = DIRECTION ( 'NONE',  ( -0.000000000000000000, -1.000000000000000000, 0.000000000000000000 ) ) ;
#2897 = VERTEX_POINT ( 'NONE', #1545 ) ;
#2898 = CARTESIAN_POINT ( 'NONE',  ( -0.3752176239131143065, 1.599166939805956034, -0.1120095174392321397 ) ) ;
#2900 = EDGE_LOOP ( 'NONE', ( #13588, #8380, #1671, #5502 ) ) ;
#2899 = DIRECTION ( 'NONE',  ( 0.000000000000000000, 0.000000000000000000, 1.000000000000000000 ) ) ;
#2901 = AXIS2_PLACEMENT_3D ( 'NONE', #8897, #11263, #834 ) ;
#2902 = EDGE_LOOP ( 'NONE', ( #354, #3331, #2256, #1269 ) ) ;
#2903 = CIRCLE ( 'NONE', #11453, 0.2944999999999998175 ) ;
#2904 = EDGE_CURVE ( 'NONE', #8207, #504, #1699, .T. ) ;
#2905 = CARTESIAN_POINT ( 'NONE',  ( 0.6592054058138496764, 0.0005989489166641660941, 0.4885496069960006404 ) ) ;
#2906 =( CONVERSION_BASED_UNIT ( 'INCH', #3052 ) LENGTH_UNIT ( ) NAMED_UNIT ( #14382 ) );
#2907 = DIRECTION ( 'NONE',  ( 0.000000000000000000, 0.000000000000000000, 1.000000000000000000 ) ) ;
#2908 = VERTEX_POINT ( 'NONE', #3864 ) ;
#2909 = VECTOR ( 'NONE', #13227, 39.37007874015748143 ) ;
#2910 = CARTESIAN_POINT ( 'NONE',  ( 2.774999999999999911, -3.360000000000016751, -0.9799999999999434719 ) ) ;
#2911 = DIRECTION ( 'NONE',  ( 0.000000000000000000, 0.000000000000000000, -1.000000000000000000 ) ) ;
#2912 = EDGE_CURVE ( 'NONE', #8918, #3698, #533, .T. ) ;
#2913 = AXIS2_PLACEMENT_3D ( 'NONE', #6564, #10927, #14582 ) ;
#2914 = DIRECTION ( 'NONE',  ( -1.000000000000000000, -0.000000000000000000, -0.000000000000000000 ) ) ;
#2915 = AXIS2_PLACEMENT_3D ( 'NONE', #12442, #5489, #14502 ) ;
#2916 = ADVANCED_FACE ( 'NONE', ( #5226 ), #6476, .F. ) ;
#2917 = CARTESIAN_POINT ( 'NONE',  ( 0.6678750254534742137, 0.02089422195403942834, 0.4666347774677351845 ) ) ;
#2918 = FACE_OUTER_BOUND ( 'NONE', #5374, .T. ) ;
#2919 = VERTEX_POINT ( 'NONE', #7448 ) ;
#2920 = CONICAL_SURFACE ( 'NONE', #14389, 0.3750000000000004996, 0.7853981633974557175 ) ;
#2921 = CARTESIAN_POINT ( 'NONE',  ( 4.344846310392954436, 3.567999999999999616, 1.491010071662831393 ) ) ;
#2922 = CARTESIAN_POINT ( 'NONE',  ( 2.774999999999999911, 1.679378605318059048, 1.973878605318042156 ) ) ;
#2923 = AXIS2_PLACEMENT_3D ( 'NONE', #5169, #4015, #8682 ) ;
#2924 = CARTESIAN_POINT ( 'NONE',  ( 0.7372049720039715037, -0.4420901695607309390, 0.4419334053338279666 ) ) ;
#2925 = FACE_OUTER_BOUND ( 'NONE', #11558, .T. ) ;
#2926 = ORIENTED_EDGE ( 'NONE', *, *, #3902, .T. ) ;
#2927 = CARTESIAN_POINT ( 'NONE',  ( -0.4999999999999996114, 1.866025403784438819, 0.000000000000000000 ) ) ;
#2928 = ORIENTED_EDGE ( 'NONE', *, *, #171, .F. ) ;
#2929 = CARTESIAN_POINT ( 'NONE',  ( 3.426491571325181340, -1.679378605318041950, 1.679378605318059048 ) ) ;
#2930 = CIRCLE ( 'NONE', #14652, 0.2624999999999852451 ) ;
#2931 = EDGE_CURVE ( 'NONE', #4332, #12765, #13314, .T. ) ;
#2932 = FACE_OUTER_BOUND ( 'NONE', #10822, .T. ) ;
#2933 = DIRECTION ( 'NONE',  ( -0.7070715176384801959, -0.7070715176384837486, -0.009986885842346790443 ) ) ;
#2934 = FACE_OUTER_BOUND ( 'NONE', #5759, .T. ) ;
#2935 = CARTESIAN_POINT ( 'NONE',  ( 1.405961592616384648, -0.05236138586009408263, -0.4801417854150228370 ) ) ;
#2936 = APPLICATION_CONTEXT ( 'automotive_design' ) ;
#2937 = CARTESIAN_POINT ( 'NONE',  ( 3.874999999999999556, 3.137999999999999901, -1.820000000000000284 ) ) ;
#2938 = VERTEX_POINT ( 'NONE', #6306 ) ;
#2939 = ORIENTED_EDGE ( 'NONE', *, *, #5112, .F. ) ;
#2940 = ORIENTED_EDGE ( 'NONE', *, *, #5610, .F. ) ;
#2941 = CARTESIAN_POINT ( 'NONE',  ( 8.775820958607647881, 0.8794096107945095220, -0.2309380233944421656 ) ) ;
#2942 = VERTEX_POINT ( 'NONE', #2784 ) ;
#2943 = DIRECTION ( 'NONE',  ( -0.7071067811865450192, 8.659560562354962440E-17, -0.7071067811865499042 ) ) ;
#2944 = DIRECTION ( 'NONE',  ( -1.000000000000000000, -0.000000000000000000, -0.000000000000000000 ) ) ;
#2945 = CARTESIAN_POINT ( 'NONE',  ( 8.475037399843312613, 0.9289129992088663856, -0.3802960819231170908 ) ) ;
#2946 = CARTESIAN_POINT ( 'NONE',  ( 4.309129212023187883, 1.779759191753760961, 0.6131832303403281781 ) ) ;
#2947 = EDGE_CURVE ( 'NONE', #9323, #1534, #9893, .T. ) ;
#2948 = ORIENTED_EDGE ( 'NONE', *, *, #10453, .T. ) ;
#2949 = ORIENTED_EDGE ( 'NONE', *, *, #8668, .T. ) ;
#2950 = ORIENTED_EDGE ( 'NONE', *, *, #5888, .T. ) ;
#2951 = ORIENTED_EDGE ( 'NONE', *, *, #9987, .T. ) ;
#2952 = VECTOR ( 'NONE', #8098, 39.37007874015748143 ) ;
#2953 = DIRECTION ( 'NONE',  ( 0.000000000000000000, 0.000000000000000000, -1.000000000000000000 ) ) ;
#2954 = DIMENSIONAL_EXPONENTS ( 1.000000000000000000, 0.000000000000000000, 0.000000000000000000, 0.000000000000000000, 0.000000000000000000, 0.000000000000000000, 0.000000000000000000 ) ;
#2955 = DIRECTION ( 'NONE',  ( -0.000000000000000000, -1.000000000000000000, -0.000000000000000000 ) ) ;
#2956 = CARTESIAN_POINT ( 'NONE',  ( 4.329787394125403921, 0.9781619162179171489, 0.2084057614748135445 ) ) ;
#2957 = DIRECTION ( 'NONE',  ( -0.000000000000000000, -1.000000000000000000, -0.000000000000000000 ) ) ;
#2958 = EDGE_LOOP ( 'NONE', ( #2240, #9012, #4322, #7072 ) ) ;
#2959 = LINE ( 'NONE', #13272, #7286 ) ;
#2960 = CARTESIAN_POINT ( 'NONE',  ( 3.338341192736666851, 2.444564215954430964, 0.5254738313631823754 ) ) ;
#2961 = ADVANCED_FACE ( 'NONE', ( #7385 ), #3935, .T. ) ;
#2962 = ADVANCED_FACE ( 'NONE', ( #10816 ), #3302, .F. ) ;
#2963 = DIRECTION ( 'NONE',  ( 0.000000000000000000, 0.000000000000000000, -1.000000000000000000 ) ) ;
#2964 = EDGE_CURVE ( 'NONE', #9941, #7401, #2061, .T. ) ;
#2965 = CIRCLE ( 'NONE', #8591, 0.06999999999999823030 ) ;
#2966 = CARTESIAN_POINT ( 'NONE',  ( 8.665761398406846894, 0.8755662462625590781, 0.3295708899401733616 ) ) ;
#2967 = CARTESIAN_POINT ( 'NONE',  ( 0.9188639271548809662, -0.4301917199507425127, -0.4641181468585011127 ) ) ;
#2968 = ADVANCED_FACE ( 'NONE', ( #2934 ), #10972, .F. ) ;
#2969 = CARTESIAN_POINT ( 'NONE',  ( 4.542752038648298907, 1.795296830498517737, 0.3463584498708582871 ) ) ;
#2971 = ORIENTED_EDGE ( 'NONE', *, *, #7389, .T. ) ;
#2970 = DIRECTION ( 'NONE',  ( 0.000000000000000000, 1.000000000000000000, 0.000000000000000000 ) ) ;
#2972 = VERTEX_POINT ( 'NONE', #12190 ) ;
#2973 = LINE ( 'NONE', #5709, #5049 ) ;
#2975 = EDGE_LOOP ( 'NONE', ( #9136, #6309 ) ) ;
#2974 = CYLINDRICAL_SURFACE ( 'NONE', #5295, 1.000000000000000000 ) ;
#2976 = VERTEX_POINT ( 'NONE', #6381 ) ;
#2977 = CARTESIAN_POINT ( 'NONE',  ( 3.426491571325181340, 2.360000000000015863, 0.9799999999999454703 ) ) ;
#2978 =( LENGTH_UNIT ( ) NAMED_UNIT ( * ) SI_UNIT ( $, .METRE. ) );
#2979 = DIRECTION ( 'NONE',  ( 1.000000000000000000, 0.000000000000000000, 0.000000000000000000 ) ) ;
#2980 = ORIENTED_EDGE ( 'NONE', *, *, #4972, .F. ) ;
#2981 = PRESENTATION_LAYER_ASSIGNMENT (  '', '', ( #6158 ) ) ;
#2982 = DIRECTION ( 'NONE',  ( 0.000000000000000000, 0.000000000000000000, -1.000000000000000000 ) ) ;
#2983 = CARTESIAN_POINT ( 'NONE',  ( 0.7513246802501660770, -0.4429999999999998939, 0.4293820849162031661 ) ) ;
#2984 = CARTESIAN_POINT ( 'NONE',  ( 3.875000000000000000, 1.059999999999999165, -0.5000000000000002220 ) ) ;
#2985 = CARTESIAN_POINT ( 'NONE',  ( 0.7009834207394378680, -0.04376407966659308368, 0.4880078140243662710 ) ) ;
#2986 = DIRECTION ( 'NONE',  ( -0.000000000000000000, -1.000000000000000000, -0.000000000000000000 ) ) ;
#2987 = ORIENTED_EDGE ( 'NONE', *, *, #8555, .F. ) ;
#2988 = CARTESIAN_POINT ( 'NONE',  ( 0.7513246802501661881, -0.5029999999999998916, -0.4293820849162031661 ) ) ;
#2989 = CARTESIAN_POINT ( 'NONE',  ( 3.760993142307637704, 1.910979010964881430, 0.4873726947928629927 ) ) ;
#2990 = CARTESIAN_POINT ( 'NONE',  ( 0.6179999999999965521, -1.679378605318047946, -1.679378605318053497 ) ) ;
#2991 = EDGE_CURVE ( 'NONE', #6614, #539, #12255, .T. ) ;
#2992 = PRODUCT_DEFINITION_SHAPE ( 'NONE', 'NONE',  #15162 ) ;
#2993 = CARTESIAN_POINT ( 'NONE',  ( 6.096491571325181269, 0.000000000000000000, -1.580000000000000071 ) ) ;
#2994 = CARTESIAN_POINT ( 'NONE',  ( 3.874999999999999556, 3.567999999999999616, -1.320000000000000062 ) ) ;
#2995 = ORIENTED_EDGE ( 'NONE', *, *, #546, .F. ) ;
#2996 = EDGE_CURVE ( 'NONE', #11615, #12467, #1766, .T. ) ;
#2997 = CARTESIAN_POINT ( 'NONE',  ( 0.09500000000000431710, -1.679378605318048390, 1.304378605318053497 ) ) ;
#2998 = ORIENTED_EDGE ( 'NONE', *, *, #5600, .F. ) ;
#2999 = SURFACE_STYLE_FILL_AREA ( #681 ) ;
#3000 = VECTOR ( 'NONE', #13226, 39.37007874015748143 ) ;
#3001 = DIRECTION ( 'NONE',  ( 0.000000000000000000, 0.000000000000000000, -1.000000000000000000 ) ) ;
#3002 = SURFACE_SIDE_STYLE ('',( #14262 ) ) ;
#3003 = DIRECTION ( 'NONE',  ( 0.000000000000000000, 0.000000000000000000, 1.000000000000000000 ) ) ;
#3004 = CARTESIAN_POINT ( 'NONE',  ( 0.9672769954795885639, -0.4829975555521404118, -0.4081482409674997980 ) ) ;
#3005 = ORIENTED_EDGE ( 'NONE', *, *, #14572, .T. ) ;
#3006 = CARTESIAN_POINT ( 'NONE',  ( 3.874999999999999556, 3.105999999999998984, -1.320000000000000062 ) ) ;
#3007 = CARTESIAN_POINT ( 'NONE',  ( 1.993429504473854585, 0.2774392468041227411, -0.4112782092410746659 ) ) ;
#3008 = DIRECTION ( 'NONE',  ( 1.000000000000000000, 0.000000000000000000, 0.000000000000000000 ) ) ;
#3009 = ORIENTED_EDGE ( 'NONE', *, *, #10175, .F. ) ;
#3010 = ORIENTED_EDGE ( 'NONE', *, *, #5456, .F. ) ;
#3011 = ADVANCED_FACE ( 'NONE', ( #9975 ), #1616, .T. ) ;
#3012 = EDGE_CURVE ( 'NONE', #2938, #13105, #6717, .T. ) ;
#3013 = FACE_OUTER_BOUND ( 'NONE', #133, .T. ) ;
#3014 = ORIENTED_EDGE ( 'NONE', *, *, #5139, .T. ) ;
#3015 = AXIS2_PLACEMENT_3D ( 'NONE', #7753, #1419, #328 ) ;
#3016 = CARTESIAN_POINT ( 'NONE',  ( 3.874999999999999556, 3.567999999999999616, 1.130000000000000560 ) ) ;
#3017 = CARTESIAN_POINT ( 'NONE',  ( 0.6742332106588940777, -0.4177279727767427842, -0.4798232997575455072 ) ) ;
#3018 = CARTESIAN_POINT ( 'NONE',  ( 2.124999999999999556, 1.575000000000016609, 1.575000000000000178 ) ) ;
#3019 = LINE ( 'NONE', #9995, #6103 ) ;
#3020 = ORIENTED_EDGE ( 'NONE', *, *, #4780, .F. ) ;
#3021 = DIRECTION ( 'NONE',  ( 0.000000000000000000, 1.000000000000000000, 0.000000000000000000 ) ) ;
#3022 = CIRCLE ( 'NONE', #4993, 0.4070000000000022489 ) ;
#3023 =( GEOMETRIC_REPRESENTATION_CONTEXT ( 3 ) GLOBAL_UNCERTAINTY_ASSIGNED_CONTEXT ( ( #7100 ) ) GLOBAL_UNIT_ASSIGNED_CONTEXT ( ( #2204, #14049, #3505 ) ) REPRESENTATION_CONTEXT ( 'NONE', 'WORKASPACE' ) );
#3024 = VERTEX_POINT ( 'NONE', #6161 ) ;
#3025 = VERTEX_POINT ( 'NONE', #11968 ) ;
#3026 = ORIENTED_EDGE ( 'NONE', *, *, #775, .F. ) ;
#3027 = DIRECTION ( 'NONE',  ( -0.000000000000000000, -1.000000000000000000, -0.000000000000000000 ) ) ;
#3028 = CARTESIAN_POINT ( 'NONE',  ( 3.426491571325181340, 0.6999999999999599876, -2.400000000000011458 ) ) ;
#3029 = DIRECTION ( 'NONE',  ( 0.000000000000000000, 0.000000000000000000, 1.000000000000000000 ) ) ;
#3030 = ITEM_DEFINED_TRANSFORMATION ( 'NONE', 'NONE', #13274,  #8424 ) ;
#3031 = DIRECTION ( 'NONE',  ( 0.000000000000000000, 0.000000000000000000, -1.000000000000000000 ) ) ;
#3032 = ORIENTED_EDGE ( 'NONE', *, *, #174, .T. ) ;
#3033 = CIRCLE ( 'NONE', #1314, 1.125000000000000888 ) ;
#3034 = DIRECTION ( 'NONE',  ( 0.000000000000000000, 0.000000000000000000, -1.000000000000000000 ) ) ;
#3035 = DIRECTION ( 'NONE',  ( -1.000000000000000000, -0.000000000000000000, -0.000000000000000000 ) ) ;
#3036 = DIRECTION ( 'NONE',  ( 0.01412288512831583534, 0.000000000000000000, 0.9999002670844989726 ) ) ;
#3037 = CARTESIAN_POINT ( 'NONE',  ( 3.874999999999999556, 3.535499999999999421, -1.509999999999999787 ) ) ;
#3038 = CYLINDRICAL_SURFACE ( 'NONE', #6505, 1.000000000000000222 ) ;
#3039 = DIRECTION ( 'NONE',  ( -0.5000000000000000000, 0.000000000000000000, 0.8660254037844385966 ) ) ;
#3040 = AXIS2_PLACEMENT_3D ( 'NONE', #2165, #4989, #6853 ) ;
#3041 = CARTESIAN_POINT ( 'NONE',  ( 4.452635031260724574, 1.784628384941731039, 0.4805815215727117229 ) ) ;
#3042 = ADVANCED_FACE ( 'NONE', ( #2713 ), #5688, .F. ) ;
#3044 = ORIENTED_EDGE ( 'NONE', *, *, #1283, .T. ) ;
#3043 = CARTESIAN_POINT ( 'NONE',  ( 3.592218582573752261, 1.983838869798021154, -0.4129877013736156788 ) ) ;
#3045 = CARTESIAN_POINT ( 'NONE',  ( 0.5400755080658357077, 0.1749999999999999889, -1.657626322880899616 ) ) ;
#3046 = ORIENTED_EDGE ( 'NONE', *, *, #3163, .T. ) ;
#3047 = EDGE_CURVE ( 'NONE', #1040, #3074, #1817, .T. ) ;
#3049 = EDGE_LOOP ( 'NONE', ( #10057, #8350, #12397, #9722 ) ) ;
#3048 = DIRECTION ( 'NONE',  ( 0.000000000000000000, 0.000000000000000000, 1.000000000000000000 ) ) ;
#3050 = ORIENTED_EDGE ( 'NONE', *, *, #3747, .T. ) ;
#3051 = FACE_BOUND ( 'NONE', #12082, .T. ) ;
#3052 = LENGTH_MEASURE_WITH_UNIT ( LENGTH_MEASURE( 0.02539999999999999897 ), #5581 );
#3053 = DIRECTION ( 'NONE',  ( 0.000000000000000000, 0.000000000000000000, -1.000000000000000000 ) ) ;
#3054 = ORIENTED_EDGE ( 'NONE', *, *, #3371, .T. ) ;
#3055 = CARTESIAN_POINT ( 'NONE',  ( 0.6179999999999965521, -1.679378605318047946, -1.304378605318053053 ) ) ;
#3056 = LINE ( 'NONE', #4286, #1655 ) ;
#3057 = EDGE_CURVE ( 'NONE', #12243, #5479, #7671, .T. ) ;
#3058 = AXIS2_PLACEMENT_3D ( 'NONE', #6888, #1042, #9030 ) ;
#3059 = AXIS2_PLACEMENT_3D ( 'NONE', #2855, #9751, #6453 ) ;
#3060 = VECTOR ( 'NONE', #14384, 39.37007874015748143 ) ;
#3061 = CARTESIAN_POINT ( 'NONE',  ( 3.082852245407359248, 0.9930332973737066027, -0.3962311736270680007 ) ) ;
#3062 = CARTESIAN_POINT ( 'NONE',  ( 2.774999999999999911, 1.679378605318059048, 1.973878605318042156 ) ) ;
#3063 = VERTEX_POINT ( 'NONE', #919 ) ;
#3064 = CARTESIAN_POINT ( 'NONE',  ( 3.874999999999999556, 3.137999999999999901, 1.098000000000000087 ) ) ;
#3065 = DIRECTION ( 'NONE',  ( -1.000000000000000000, -0.000000000000000000, -0.000000000000000000 ) ) ;
#3066 = CARTESIAN_POINT ( 'NONE',  ( 3.375824834555410270, 0.9995867961477209462, 0.03321238156889033677 ) ) ;
#3067 = ADVANCED_FACE ( 'NONE', ( #9056 ), #10872, .F. ) ;
#3068 = CARTESIAN_POINT ( 'NONE',  ( 4.271198831181767908, 1.710003382540315808, -0.6913879080909109964 ) ) ;
#3069 = ORIENTED_EDGE ( 'NONE', *, *, #617, .T. ) ;
#3070 = AXIS2_PLACEMENT_3D ( 'NONE', #13091, #9447, #4772 ) ;
#3071 = EDGE_CURVE ( 'NONE', #10523, #14399, #4774, .T. ) ;
#3072 = CARTESIAN_POINT ( 'NONE',  ( 0.7034818293080725704, -0.4179380312349338933, 0.4790337915202410590 ) ) ;
#3073 = LINE ( 'NONE', #452, #13321 ) ;
#3074 = VERTEX_POINT ( 'NONE', #6762 ) ;
#3075 = VECTOR ( 'NONE', #7575, 39.37007874015748143 ) ;
#3076 = AXIS2_PLACEMENT_3D ( 'NONE', #8285, #6976, #2137 ) ;
#3077 = DIRECTION ( 'NONE',  ( -0.03489949670249409275, 0.9993908270190960952, 0.000000000000000000 ) ) ;
#3078 = ORIENTED_EDGE ( 'NONE', *, *, #7093, .T. ) ;
#3079 =( NAMED_UNIT ( * ) SI_UNIT ( $, .STERADIAN. ) SOLID_ANGLE_UNIT ( ) );
#3080 = CARTESIAN_POINT ( 'NONE',  ( 2.634365942216866596, 0.3629388174706745240, -0.4627914414941119992 ) ) ;
#3081 = CARTESIAN_POINT ( 'NONE',  ( 3.492022057095982568, 2.024959266993827889, -0.6451503923273511631 ) ) ;
#3082 = EDGE_CURVE ( 'NONE', #12843, #6091, #11609, .T. ) ;
#3083 = VECTOR ( 'NONE', #6746, 39.37007874015748143 ) ;
#3084 = CARTESIAN_POINT ( 'NONE',  ( 0.3724999999999997757, 0.1859999999999983611, -0.3725000000000000533 ) ) ;
#3085 = CARTESIAN_POINT ( 'NONE',  ( 2.774999999999999911, 0.000000000000000000, 0.000000000000000000 ) ) ;
#3086 = AXIS2_PLACEMENT_3D ( 'NONE', #1052, #14060, #11549 ) ;
#3087 = CIRCLE ( 'NONE', #10159, 0.3750000000000004996 ) ;
#3088 = ADVANCED_FACE ( 'NONE', ( #8827 ), #1566, .F. ) ;
#3089 = ORIENTED_EDGE ( 'NONE', *, *, #9889, .F. ) ;
#3090 = DIRECTION ( 'NONE',  ( -0.000000000000000000, 1.000000000000000000, -0.000000000000000000 ) ) ;
#3091 = CARTESIAN_POINT ( 'NONE',  ( 3.587393574774031979, 1.880815582072911551, 0.7577781223979582759 ) ) ;
#3092 = DIRECTION ( 'NONE',  ( -0.000000000000000000, -1.000000000000000000, -0.000000000000000000 ) ) ;
#3093 = ORIENTED_EDGE ( 'NONE', *, *, #1950, .T. ) ;
#3094 = ORIENTED_EDGE ( 'NONE', *, *, #8858, .F. ) ;
#3095 = CARTESIAN_POINT ( 'NONE',  ( 2.774999999999999911, 1.679378605318042395, -1.973878605318057478 ) ) ;
#3096 = VERTEX_POINT ( 'NONE', #14859 ) ;
#3097 = DIRECTION ( 'NONE',  ( -0.000000000000000000, -1.000000000000000000, -0.000000000000000000 ) ) ;
#3098 = EDGE_CURVE ( 'NONE', #13120, #5891, #5753, .T. ) ;
#3099 = CARTESIAN_POINT ( 'NONE',  ( 2.124999999999999556, -0.6999999999999990674, -2.399999999999999911 ) ) ;
#3100 = CARTESIAN_POINT ( 'NONE',  ( 0.9173974589322090312, -0.4301166320577336499, -0.4642204989205186427 ) ) ;
#3101 = CARTESIAN_POINT ( 'NONE',  ( 4.525278585568729639, 1.792793477108324485, -0.3771970452947643881 ) ) ;
#3102 = EDGE_CURVE ( 'NONE', #3626, #7297, #12332, .T. ) ;
#3103 = EDGE_CURVE ( 'NONE', #9683, #13623, #7695, .T. ) ;
#3104 = AXIS2_PLACEMENT_3D ( 'NONE', #8331, #5786, #12962 ) ;
#3105 = VERTEX_POINT ( 'NONE', #7898 ) ;
#3106 = DIRECTION ( 'NONE',  ( 0.000000000000000000, 0.000000000000000000, -1.000000000000000000 ) ) ;
#3107 = VECTOR ( 'NONE', #3811, 39.37007874015748143 ) ;
#3108 = ORIENTED_EDGE ( 'NONE', *, *, #5685, .F. ) ;
#3109 = ORIENTED_EDGE ( 'NONE', *, *, #8595, .T. ) ;
#3110 = PRODUCT_DEFINITION_CONTEXT ( 'detailed design', #3426, 'design' ) ;
#3111 = ORIENTED_EDGE ( 'NONE', *, *, #5141, .T. ) ;
#3112 = CARTESIAN_POINT ( 'NONE',  ( 3.921022896101461708, 1.873041151412256911, -0.4984237362096384794 ) ) ;
#3113 = DIRECTION ( 'NONE',  ( -1.000000000000000000, 0.000000000000000000, -1.224646799147353207E-16 ) ) ;
#3114 = CARTESIAN_POINT ( 'NONE',  ( 2.124999999999999556, -2.400000000000011902, -0.6999999999999596545 ) ) ;
#3115 = AXIS2_PLACEMENT_3D ( 'NONE', #541, #6314, #8548 ) ;
#3116 = CARTESIAN_POINT ( 'NONE',  ( 3.874999999999999556, 3.105999999999998984, -1.320000000000000062 ) ) ;
#3117 = VERTEX_POINT ( 'NONE', #11416 ) ;
#3118 = DIRECTION ( 'NONE',  ( -1.000000000000000000, -0.000000000000000000, -0.000000000000000000 ) ) ;
#3119 = CARTESIAN_POINT ( 'NONE',  ( 6.794491571325181667, 1.679378605318059492, 1.679378605318041506 ) ) ;
#3120 = DIRECTION ( 'NONE',  ( 1.000000000000000000, 0.000000000000000000, 0.000000000000000000 ) ) ;
#3121 = CARTESIAN_POINT ( 'NONE',  ( 0.000000000000000000, 1.559103846021539619, 0.000000000000000000 ) ) ;
#3122 = AXIS2_PLACEMENT_3D ( 'NONE', #7409, #3894, #1573 ) ;
#3123 = EDGE_CURVE ( 'NONE', #14371, #5452, #1088, .T. ) ;
#3124 = CARTESIAN_POINT ( 'NONE',  ( 8.775820958607726041, 0.8794096107943684126, 0.2309380233943977012 ) ) ;
#3125 = CARTESIAN_POINT ( 'NONE',  ( 0.000000000000000000, 1.159999999999999698, 0.000000000000000000 ) ) ;
#3126 = CARTESIAN_POINT ( 'NONE',  ( 4.116403661786756096, 1.796907475018162392, 0.7114969261561383540 ) ) ;
#3128 = EDGE_LOOP ( 'NONE', ( #6619, #14044, #9370, #13549 ) ) ;
#3127 = CARTESIAN_POINT ( 'NONE',  ( 3.759442893977343658, 1.920756169463178509, -0.4870029225387685345 ) ) ;
#3129 = AXIS2_PLACEMENT_3D ( 'NONE', #7163, #15, #8238 ) ;
#3130 = VERTEX_POINT ( 'NONE', #6531 ) ;
#3132 = VERTEX_POINT ( 'NONE', #13768 ) ;
#3131 = CARTESIAN_POINT ( 'NONE',  ( -0.3725000000000000533, -0.6290000000000005587, 0.4124999999999999223 ) ) ;
#3133 = VERTEX_POINT ( 'NONE', #837 ) ;
#3134 = AXIS2_PLACEMENT_3D ( 'NONE', #4431, #12680, #8948 ) ;
#3135 = CYLINDRICAL_SURFACE ( 'NONE', #3369, 0.3750000000000007772 ) ;
#3136 = CARTESIAN_POINT ( 'NONE',  ( 2.124999999999999556, 1.679378605318042395, -1.679378605318058604 ) ) ;
#3137 = VERTEX_POINT ( 'NONE', #5460 ) ;
#3138 = CYLINDRICAL_SURFACE ( 'NONE', #13116, 0.7849999999999998090 ) ;
#3139 = FACE_OUTER_BOUND ( 'NONE', #10716, .T. ) ;
#3140 = VECTOR ( 'NONE', #2495, 39.37007874015748143 ) ;
#3141 = DIRECTION ( 'NONE',  ( -1.000000000000000000, -0.000000000000000000, -0.000000000000000000 ) ) ;
#3142 = CARTESIAN_POINT ( 'NONE',  ( 0.2249147617188371751, 1.239999999999999991, -0.3723417112827391295 ) ) ;
#3143 = VECTOR ( 'NONE', #11016, 39.37007874015748143 ) ;
#3144 = CARTESIAN_POINT ( 'NONE',  ( 2.599116034107009199, 0.7926631980424555524, -0.4028586330192087672 ) ) ;
#3145 = PRODUCT_RELATED_PRODUCT_CATEGORY ( 'part', '', ( #1752 ) ) ;
#3146 = CARTESIAN_POINT ( 'NONE',  ( 0.9747900039790298177, -0.4432332186376475303, -0.3667232257088772207 ) ) ;
#3147 = ORIENTED_EDGE ( 'NONE', *, *, #8767, .F. ) ;
#3148 = DIRECTION ( 'NONE',  ( 2.602462600580852055E-17, 1.000000000000000000, -0.000000000000000000 ) ) ;
#3149 = CIRCLE ( 'NONE', #4868, 0.4070000000000046914 ) ;
#3150 = CARTESIAN_POINT ( 'NONE',  ( 3.532925020153219631, 0.9310773776131279211, -0.3650227795079680759 ) ) ;
#3151 = AXIS2_PLACEMENT_3D ( 'NONE', #9677, #2933, #11035 ) ;
#3152 = CARTESIAN_POINT ( 'NONE',  ( 3.629047196404351805, 1.863650056189079418, -0.7701527217475101494 ) ) ;
#3153 = CIRCLE ( 'NONE', #6096, 0.2624999999999852451 ) ;
#3154 = CARTESIAN_POINT ( 'NONE',  ( 0.000000000000000000, 1.249999999999999778, -0.3190000000000000058 ) ) ;
#3155 = DIRECTION ( 'NONE',  ( -0.7070715176384816392, -0.7070715176384821943, 0.009986885842350832349 ) ) ;
#3156 = ORIENTED_EDGE ( 'NONE', *, *, #1876, .T. ) ;
#3157 = AXIS2_PLACEMENT_3D ( 'NONE', #2740, #3746, #3816 ) ;
#3158 = DIRECTION ( 'NONE',  ( 1.000000000000000000, 0.000000000000000000, 0.000000000000000000 ) ) ;
#3159 = CIRCLE ( 'NONE', #8310, 0.7500000000000001110 ) ;
#3160 = VERTEX_POINT ( 'NONE', #10127 ) ;
#3161 = VECTOR ( 'NONE', #4672, 39.37007874015748143 ) ;
#3162 = EDGE_CURVE ( 'NONE', #9653, #3646, #10141, .T. ) ;
#3163 = EDGE_CURVE ( 'NONE', #13167, #2708, #13469, .T. ) ;
#3164 = CARTESIAN_POINT ( 'NONE',  ( 0.4349147617188415249, 1.559103846021539619, 0.008611041693268213504 ) ) ;
#3165 = FACE_OUTER_BOUND ( 'NONE', #5079, .T. ) ;
#3166 = EDGE_CURVE ( 'NONE', #12504, #12651, #14034, .T. ) ;
#3167 = DIRECTION ( 'NONE',  ( 0.000000000000000000, 0.000000000000000000, -1.000000000000000000 ) ) ;
#3168 = AXIS2_PLACEMENT_3D ( 'NONE', #4471, #3181, #12489 ) ;
#3169 = VERTEX_POINT ( 'NONE', #691 ) ;
#3170 = CARTESIAN_POINT ( 'NONE',  ( 2.774999999999999911, -1.679378605318059048, -1.973878605318027724 ) ) ;
#3171 = CARTESIAN_POINT ( 'NONE',  ( 1.375000000000000000, 1.653273178848927113E-16, -1.350000000000000089 ) ) ;
#3172 = EDGE_CURVE ( 'NONE', #12462, #2380, #10052, .T. ) ;
#3173 = CARTESIAN_POINT ( 'NONE',  ( 0.7238317330277980188, -0.4379309809303465473, -0.4548041668469362531 ) ) ;
#3174 = ORIENTED_EDGE ( 'NONE', *, *, #3071, .F. ) ;
#3175 = VERTEX_POINT ( 'NONE', #12409 ) ;
#3176 = CARTESIAN_POINT ( 'NONE',  ( 0.3724999999999999423, 0.1859999999999983611, 0.4124999999999999223 ) ) ;
#3177 = ORIENTED_EDGE ( 'NONE', *, *, #2500, .T. ) ;
#3178 = CARTESIAN_POINT ( 'NONE',  ( 1.249152626892299001, 0.000000000000000000, 0.4223506167432916625 ) ) ;
#3179 = CARTESIAN_POINT ( 'NONE',  ( 2.230477600021715467, 0.4287871555018996084, 0.4684960790957384824 ) ) ;
#3180 = AXIS2_PLACEMENT_3D ( 'NONE', #6302, #10966, #11546 ) ;
#3181 = DIRECTION ( 'NONE',  ( -1.365923996832131609E-16, 1.000000000000000000, -0.000000000000000000 ) ) ;
#3182 = DIRECTION ( 'NONE',  ( -0.000000000000000000, -1.000000000000000000, -0.000000000000000000 ) ) ;
#3183 = ORIENTED_EDGE ( 'NONE', *, *, #5627, .T. ) ;
#3184 = AXIS2_PLACEMENT_3D ( 'NONE', #14283, #14210, #5047 ) ;
#3185 = VERTEX_POINT ( 'NONE', #7749 ) ;
#3186 = ORIENTED_EDGE ( 'NONE', *, *, #3057, .T. ) ;
#3187 = ADVANCED_FACE ( 'NONE', ( #11265 ), #7451, .F. ) ;
#3188 = VERTEX_POINT ( 'NONE', #161 ) ;
#3189 = CARTESIAN_POINT ( 'NONE',  ( 3.944129661530210385, 1.867491090171841339, -0.4951980309903490363 ) ) ;
#3190 = CARTESIAN_POINT ( 'NONE',  ( 3.426491571325181340, 0.000000000000000000, 0.000000000000000000 ) ) ;
#3191 = CARTESIAN_POINT ( 'NONE',  ( 0.7997892116363007897, -0.4435060640070847549, -0.3079891465263297490 ) ) ;
#3192 = EDGE_CURVE ( 'NONE', #12451, #1686, #13294, .T. ) ;
#3193 = CARTESIAN_POINT ( 'NONE',  ( -0.1702344636782962828, 1.581111061277888252, 0.3809527529760087239 ) ) ;
#3194 = ORIENTED_EDGE ( 'NONE', *, *, #7003, .T. ) ;
#3195 = CARTESIAN_POINT ( 'NONE',  ( 3.129894412017060201, 2.499001391242224202, -0.07213773670819455253 ) ) ;
#3196 = CARTESIAN_POINT ( 'NONE',  ( 0.7009701624870741110, -0.04368263270409020876, -0.4879883456728131841 ) ) ;
#3197 = CARTESIAN_POINT ( 'NONE',  ( 0.9431121448573139832, -0.4733191448316948491, -0.4367219098727821436 ) ) ;
#3198 = CIRCLE ( 'NONE', #6872, 0.03999999999999998002 ) ;
#3199 = CARTESIAN_POINT ( 'NONE',  ( 3.932805631546712810, 1.785024703590347261, 0.7488574126153495492 ) ) ;
#3201 = ORIENTED_EDGE ( 'NONE', *, *, #11142, .T. ) ;
#3200 = CARTESIAN_POINT ( 'NONE',  ( 6.176491571325181340, -1.679378605318047946, -2.086378605318055968 ) ) ;
#3202 = ORIENTED_EDGE ( 'NONE', *, *, #14617, .T. ) ;
#3204 = ORIENTED_EDGE ( 'NONE', *, *, #12724, .F. ) ;
#3203 = FACE_BOUND ( 'NONE', #6181, .T. ) ;
#3205 = VERTEX_POINT ( 'NONE', #5699 ) ;
#3206 = FACE_BOUND ( 'NONE', #5790, .T. ) ;
#3207 = EDGE_CURVE ( 'NONE', #11406, #1865, #10358, .T. ) ;
#3208 = CARTESIAN_POINT ( 'NONE',  ( 0.000000000000000000, 1.559103846021539619, 0.000000000000000000 ) ) ;
#3209 = ORIENTED_EDGE ( 'NONE', *, *, #5326, .F. ) ;
#3210 = DIRECTION ( 'NONE',  ( 0.000000000000000000, 0.000000000000000000, 1.000000000000000000 ) ) ;
#3211 = CARTESIAN_POINT ( 'NONE',  ( -5.764454660286586870E-18, 0.04143956043956045082, 0.000000000000000000 ) ) ;
#3212 = CONICAL_SURFACE ( 'NONE', #6393, 0.2944999999999856066, 0.7853981633974514986 ) ;
#3213 = CARTESIAN_POINT ( 'NONE',  ( 3.394491571325180423, -1.679378605318059048, -1.679378605318041950 ) ) ;
#3214 = CARTESIAN_POINT ( 'NONE',  ( 2.156999999999999584, 1.679378605318059048, 1.416878605318041773 ) ) ;
#3215 = CARTESIAN_POINT ( 'NONE',  ( 0.9672649160634322341, -0.4430530727333171770, -0.4081727571047791825 ) ) ;
#3216 = EDGE_LOOP ( 'NONE', ( #10092, #7677, #14280, #12469 ) ) ;
#3217 = FACE_OUTER_BOUND ( 'NONE', #6637, .T. ) ;
#3218 = CARTESIAN_POINT ( 'NONE',  ( 3.448855552202333197, 1.982883164696786382, 0.2625902165005476463 ) ) ;
#3219 = LINE ( 'NONE', #821, #5009 ) ;
#3220 = AXIS2_PLACEMENT_3D ( 'NONE', #993, #7979, #832 ) ;
#3221 = DIRECTION ( 'NONE',  ( 0.000000000000000000, 0.000000000000000000, -1.000000000000000000 ) ) ;
#3223 = ORIENTED_EDGE ( 'NONE', *, *, #15069, .T. ) ;
#3222 = DIRECTION ( 'NONE',  ( 0.000000000000000000, 0.000000000000000000, 1.000000000000000000 ) ) ;
#3224 = ORIENTED_EDGE ( 'NONE', *, *, #14852, .T. ) ;
#3225 = CARTESIAN_POINT ( 'NONE',  ( 2.774999999999999911, -2.400000000000011902, -0.6999999999999596545 ) ) ;
#3226 = EDGE_LOOP ( 'NONE', ( #5403, #13145, #4222, #14376 ) ) ;
#3227 = ADVANCED_FACE ( 'NONE', ( #3632 ), #6994, .F. ) ;
#3228 = CYLINDRICAL_SURFACE ( 'NONE', #7332, 0.9499999999999992895 ) ;
#3229 = FACE_OUTER_BOUND ( 'NONE', #2294, .T. ) ;
#3230 = DIRECTION ( 'NONE',  ( -0.000000000000000000, -1.000000000000000000, -0.000000000000000000 ) ) ;
#3231 = FACE_OUTER_BOUND ( 'NONE', #14748, .T. ) ;
#3232 = ORIENTED_EDGE ( 'NONE', *, *, #2064, .T. ) ;
#3233 = DIRECTION ( 'NONE',  ( -1.000000000000000000, -0.000000000000000000, -0.000000000000000000 ) ) ;
#3234 = DIRECTION ( 'NONE',  ( 1.655665450705613915E-16, 0.000000000000000000, 1.000000000000000000 ) ) ;
#3235 = CARTESIAN_POINT ( 'NONE',  ( 3.874999999999999556, 3.170500000000000096, 1.320000000000000062 ) ) ;
#3236 = ORIENTED_EDGE ( 'NONE', *, *, #6439, .F. ) ;
#3237 = EDGE_CURVE ( 'NONE', #1686, #12451, #14304, .T. ) ;
#3238 = EDGE_CURVE ( 'NONE', #6179, #8878, #4860, .T. ) ;
#3239 = DIRECTION ( 'NONE',  ( -1.000000000000000000, -0.000000000000000000, -0.000000000000000000 ) ) ;
#3240 = ORIENTED_EDGE ( 'NONE', *, *, #198, .F. ) ;
#3241 = EDGE_CURVE ( 'NONE', #11167, #12941, #3851, .T. ) ;
#3242 = DIRECTION ( 'NONE',  ( -1.000000000000000000, 0.000000000000000000, -0.000000000000000000 ) ) ;
#3243 = CARTESIAN_POINT ( 'NONE',  ( 0.6782188896242887788, -0.4297562849107281480, -0.4691064452754618586 ) ) ;
#3244 = CARTESIAN_POINT ( 'NONE',  ( 0.9936287706375830364, -0.4425130709408415242, -0.4361110481179421017 ) ) ;
#3245 = ADVANCED_FACE ( 'NONE', ( #5857 ), #4548, .F. ) ;
#3246 = CARTESIAN_POINT ( 'NONE',  ( 3.875000000000000000, 1.885381157978845312, 0.5000000000000002220 ) ) ;
#3247 = VECTOR ( 'NONE', #11037, 39.37007874015748143 ) ;
#3248 = ORIENTED_EDGE ( 'NONE', *, *, #46, .T. ) ;
#3249 = VECTOR ( 'NONE', #13628, 39.37007874015748854 ) ;
#3250 = CARTESIAN_POINT ( 'NONE',  ( 3.671600895815123167, 1.871391630887606405, -0.7219642105703503177 ) ) ;
#3251 = ORIENTED_EDGE ( 'NONE', *, *, #9336, .F. ) ;
#3252 = EDGE_CURVE ( 'NONE', #9941, #1198, #4628, .T. ) ;
#3253 = ORIENTED_EDGE ( 'NONE', *, *, #8668, .F. ) ;
#3254 = PRODUCT_DEFINITION_CONTEXT ( 'detailed design', #8901, 'design' ) ;
#3255 = CARTESIAN_POINT ( 'NONE',  ( 2.774999999999999911, -0.9799999999999986500, -3.359999999999999876 ) ) ;
#3256 = ORIENTED_EDGE ( 'NONE', *, *, #14216, .T. ) ;
#3257 = CARTESIAN_POINT ( 'NONE',  ( -0.4349147617188415249, 1.239999999999999991, 0.008611041693274120237 ) ) ;
#3258 = LINE ( 'NONE', #13798, #4330 ) ;
#3259 = CARTESIAN_POINT ( 'NONE',  ( 0.7867468462925758521, -0.4450678903015412580, -0.3210486967726864371 ) ) ;
#3260 = FACE_OUTER_BOUND ( 'NONE', #10345, .T. ) ;
#3261 = VERTEX_POINT ( 'NONE', #9218 ) ;
#3262 = DIRECTION ( 'NONE',  ( 0.000000000000000000, 0.000000000000000000, 1.000000000000000000 ) ) ;
#3263 = CARTESIAN_POINT ( 'NONE',  ( 0.6894183887957242574, 0.0001162156558598427650, -0.4464953827605273040 ) ) ;
#3264 = CIRCLE ( 'NONE', #12295, 0.03999999999999998002 ) ;
#3265 = CARTESIAN_POINT ( 'NONE',  ( 3.394491571325182644, 1.679378605318042395, -1.679378605318058604 ) ) ;
#3266 = EDGE_CURVE ( 'NONE', #4777, #2897, #8213, .T. ) ;
#3267 = CIRCLE ( 'NONE', #8884, 0.3750000000000004996 ) ;
#3268 = DIRECTION ( 'NONE',  ( 0.000000000000000000, 1.000000000000000000, 0.000000000000000000 ) ) ;
#3269 = EDGE_CURVE ( 'NONE', #9046, #12211, #1239, .T. ) ;
#3270 = CARTESIAN_POINT ( 'NONE',  ( 3.945347773489349397, 1.834617440766652230, 0.7476453199387252946 ) ) ;
#3272 = VERTEX_POINT ( 'NONE', #9453 ) ;
#3271 = CARTESIAN_POINT ( 'NONE',  ( 2.774999999999999911, -3.360000000000000320, 0.9799999999999999822 ) ) ;
#3273 = ORIENTED_EDGE ( 'NONE', *, *, #15130, .F. ) ;
#3274 = CIRCLE ( 'NONE', #320, 1.039370078740158965 ) ;
#3276 = ORIENTED_EDGE ( 'NONE', *, *, #889, .T. ) ;
#3275 = FACE_OUTER_BOUND ( 'NONE', #3762, .T. ) ;
#3277 = ORIENTED_EDGE ( 'NONE', *, *, #12305, .F. ) ;
#3278 =( GEOMETRIC_REPRESENTATION_CONTEXT ( 3 ) GLOBAL_UNCERTAINTY_ASSIGNED_CONTEXT ( ( #945 ) ) GLOBAL_UNIT_ASSIGNED_CONTEXT ( ( #5734, #11774, #6807 ) ) REPRESENTATION_CONTEXT ( 'NONE', 'WORKASPACE' ) );
#3279 = ADVANCED_BREP_SHAPE_REPRESENTATION ( '', ( #5275, #8424 ), #10122 ) ;
#3280 = CARTESIAN_POINT ( 'NONE',  ( 2.775039370078740131, 1.679378605318035733, -1.679378605318065487 ) ) ;
#3281 =( LENGTH_UNIT ( ) NAMED_UNIT ( * ) SI_UNIT ( $, .METRE. ) );
#3282 = CARTESIAN_POINT ( 'NONE',  ( 2.775039370078740131, -1.679378605318048390, 1.304378605318053497 ) ) ;
#3283 = ORIENTED_EDGE ( 'NONE', *, *, #2801, .F. ) ;
#3284 = CARTESIAN_POINT ( 'NONE',  ( 0.06299999999999994493, -1.679378605318047946, -2.086378605318059076 ) ) ;
#3285 = CARTESIAN_POINT ( 'NONE',  ( 0.6558056096843536409, -0.4243327889391083074, -0.5013356986195880438 ) ) ;
#3286 = CARTESIAN_POINT ( 'NONE',  ( 2.774999999999999911, -1.575000000000016387, -2.359999999999999876 ) ) ;
#3287 = CARTESIAN_POINT ( 'NONE',  ( 3.340400805682919305, 1.044207302811546612, -0.4528191976596157020 ) ) ;
#3288 = CARTESIAN_POINT ( 'NONE',  ( 2.774999999999999911, -0.9799999999999990941, -2.359999999999999876 ) ) ;
#3289 = PRODUCT_DEFINITION_FORMATION_WITH_SPECIFIED_SOURCE ( 'ANY', '', #12392, .NOT_KNOWN. ) ;
#3290 = CYLINDRICAL_SURFACE ( 'NONE', #12054, 0.2625000000000000111 ) ;
#3291 = EDGE_CURVE ( 'NONE', #1348, #6530, #10648, .T. ) ;
#3292 = DIRECTION ( 'NONE',  ( 0.000000000000000000, -1.000000000000000000, -0.000000000000000000 ) ) ;
#3293 = CARTESIAN_POINT ( 'NONE',  ( 3.875000000000000000, 0.8660254037844385966, -0.5000000000000002220 ) ) ;
#3294 = LINE ( 'NONE', #12465, #13271 ) ;
#3295 = DIRECTION ( 'NONE',  ( 0.000000000000000000, 0.000000000000000000, -1.000000000000000000 ) ) ;
#3297 = EDGE_LOOP ( 'NONE', ( #4396, #4217 ) ) ;
#3296 = CARTESIAN_POINT ( 'NONE',  ( -0.4125000000000000333, 0.1859999999999983611, 0.4124999999999999223 ) ) ;
#3298 = ORIENTED_EDGE ( 'NONE', *, *, #1028, .T. ) ;
#3299 = DIRECTION ( 'NONE',  ( 0.000000000000000000, -1.000000000000000000, 0.000000000000000000 ) ) ;
#3300 = ORIENTED_EDGE ( 'NONE', *, *, #4420, .F. ) ;
#3301 = DIRECTION ( 'NONE',  ( 0.000000000000000000, 0.000000000000000000, -1.000000000000000000 ) ) ;
#3302 = CONICAL_SURFACE ( 'NONE', #4026, 0.2225000000000012523, 0.7853981633974446153 ) ;
#3303 = AXIS2_PLACEMENT_3D ( 'NONE', #12404, #6608, #4387 ) ;
#3304 = LINE ( 'NONE', #12625, #4253 ) ;
#3305 = CARTESIAN_POINT ( 'NONE',  ( 2.002892399652359323, -0.1783233198217482329, 0.4717105593267386654 ) ) ;
#3306 = FACE_OUTER_BOUND ( 'NONE', #12101, .T. ) ;
#3307 = CARTESIAN_POINT ( 'NONE',  ( -0.4125000000000001998, -0.6290000000000005587, -0.4125000000000000333 ) ) ;
#3308 = LINE ( 'NONE', #6609, #8763 ) ;
#3309 = VERTEX_POINT ( 'NONE', #14015 ) ;
#3310 = ADVANCED_FACE ( 'NONE', ( #2169, #9300 ), #10435, .T. ) ;
#3311 = DIRECTION ( 'NONE',  ( 0.000000000000000000, 0.000000000000000000, -1.000000000000000000 ) ) ;
#3312 = CARTESIAN_POINT ( 'NONE',  ( 0.8395338176367566074, -0.4829999999999997629, -0.3304795099493806343 ) ) ;
#3313 = VECTOR ( 'NONE', #12303, 39.37007874015748143 ) ;
#3314 = AXIS2_PLACEMENT_3D ( 'NONE', #9191, #8053, #12928 ) ;
#3315 = ORIENTED_EDGE ( 'NONE', *, *, #14833, .T. ) ;
#3316 = FACE_OUTER_BOUND ( 'NONE', #13552, .T. ) ;
#3317 = ORIENTED_EDGE ( 'NONE', *, *, #1801, .F. ) ;
#3318 = CARTESIAN_POINT ( 'NONE',  ( 0.8999999999999998002, 0.000000000000000000, -0.3799999999999999489 ) ) ;
#3319 = CARTESIAN_POINT ( 'NONE',  ( 0.000000000000000000, 4.529999999999999361, 0.000000000000000000 ) ) ;
#3320 = ORIENTED_EDGE ( 'NONE', *, *, #3528, .T. ) ;
#3321 = DIRECTION ( 'NONE',  ( -1.000000000000000000, -0.000000000000000000, -0.000000000000000000 ) ) ;
#3322 = DIRECTION ( 'NONE',  ( -0.7071067811865441310, 0.000000000000000000, 0.7071067811865509034 ) ) ;
#3323 = CYLINDRICAL_SURFACE ( 'NONE', #5123, 0.5000000000000001110 ) ;
#3324 = CIRCLE ( 'NONE', #9196, 0.3803340137431718282 ) ;
#3325 = CARTESIAN_POINT ( 'NONE',  ( 2.774999999999999911, 1.679378605318059048, 1.384878605318040856 ) ) ;
#3326 = EDGE_CURVE ( 'NONE', #14534, #9554, #12099, .T. ) ;
#3327 = VECTOR ( 'NONE', #9579, 39.37007874015748143 ) ;
#3328 = ORIENTED_EDGE ( 'NONE', *, *, #9735, .F. ) ;
#3329 = ORIENTED_EDGE ( 'NONE', *, *, #14090, .F. ) ;
#3330 = DIRECTION ( 'NONE',  ( -1.000000000000000000, -0.000000000000000000, -0.000000000000000000 ) ) ;
#3331 = ORIENTED_EDGE ( 'NONE', *, *, #11087, .F. ) ;
#3332 = DIRECTION ( 'NONE',  ( 0.000000000000000000, 1.000000000000000000, 4.591341165822158293E-16 ) ) ;
#3333 = CYLINDRICAL_SURFACE ( 'NONE', #11161, 0.2812500000000000555 ) ;
#3334 = DIRECTION ( 'NONE',  ( 0.000000000000000000, 0.000000000000000000, -1.000000000000000000 ) ) ;
#3335 = DIRECTION ( 'NONE',  ( 0.000000000000000000, 0.000000000000000000, 1.000000000000000000 ) ) ;
#3336 = ORIENTED_EDGE ( 'NONE', *, *, #1738, .F. ) ;
#3337 = CARTESIAN_POINT ( 'NONE',  ( 3.126632629065664748, 2.499978424780176400, 0.05909466466767844539 ) ) ;
#3338 = CARTESIAN_POINT ( 'NONE',  ( 0.6592465977460930660, 0.0007463589180138885653, -0.4884267951992124490 ) ) ;
#3339 = DIRECTION ( 'NONE',  ( -0.000000000000000000, 1.000000000000000000, -0.000000000000000000 ) ) ;
#3340 = ADVANCED_FACE ( 'NONE', ( #8152 ), #5771, .F. ) ;
#3341 = ADVANCED_FACE ( 'NONE', ( #12870 ), #2402, .F. ) ;
#3342 = EDGE_CURVE ( 'NONE', #13623, #9683, #6736, .T. ) ;
#3343 = AXIS2_PLACEMENT_3D ( 'NONE', #9483, #6959, #3740 ) ;
#3344 = FACE_OUTER_BOUND ( 'NONE', #11274, .T. ) ;
#3345 = CARTESIAN_POINT ( 'NONE',  ( 4.586364424524735028, 1.743277076888124277, 0.2448609443050739909 ) ) ;
#3346 = ORIENTED_EDGE ( 'NONE', *, *, #10083, .T. ) ;
#3348 = ORIENTED_EDGE ( 'NONE', *, *, #12591, .T. ) ;
#3347 = CARTESIAN_POINT ( 'NONE',  ( 0.3389861398596112907, 1.603403919227001095, 0.1747642886535209217 ) ) ;
#3349 = ADVANCED_FACE ( 'NONE', ( #6503 ), #579, .T. ) ;
#3350 = AXIS2_PLACEMENT_3D ( 'NONE', #6633, #10224, #12277 ) ;
#3351 = ORIENTED_EDGE ( 'NONE', *, *, #7380, .F. ) ;
#3353 = EDGE_LOOP ( 'NONE', ( #9115, #10416, #2824, #10004, #9741, #1172, #13864, #8449, #2017 ) ) ;
#3352 = DIRECTION ( 'NONE',  ( 0.000000000000000000, 0.000000000000000000, -1.000000000000000000 ) ) ;
#3354 = ORIENTED_EDGE ( 'NONE', *, *, #14522, .T. ) ;
#3355 = EDGE_CURVE ( 'NONE', #15055, #15129, #108, .T. ) ;
#3356 = CARTESIAN_POINT ( 'NONE',  ( 6.176491571325181340, 1.679378605318035733, -2.086378605318067958 ) ) ;
#3357 = CARTESIAN_POINT ( 'NONE',  ( 0.000000000000000000, 0.000000000000000000, 0.000000000000000000 ) ) ;
#3358 = EDGE_LOOP ( 'NONE', ( #1266, #9044, #13835, #11931 ) ) ;
#3359 = DIRECTION ( 'NONE',  ( 0.000000000000000000, 0.000000000000000000, -1.000000000000000000 ) ) ;
#3360 = CARTESIAN_POINT ( 'NONE',  ( 0.6940366006580477309, -0.4844395604395604349, -0.4146323121508169729 ) ) ;
#3361 = VECTOR ( 'NONE', #8853, 39.37007874015748143 ) ;
#3362 = CARTESIAN_POINT ( 'NONE',  ( 3.874999999999999556, 3.137999999999999901, -1.320000000000000062 ) ) ;
#3363 = DIRECTION ( 'NONE',  ( -0.000000000000000000, -1.000000000000000000, -0.000000000000000000 ) ) ;
#3364 = CARTESIAN_POINT ( 'NONE',  ( 1.564978703518703940, 0.1749999999999999889, -0.4193347797797316034 ) ) ;
#3365 = CIRCLE ( 'NONE', #1644, 0.3190000000000000058 ) ;
#3366 = CARTESIAN_POINT ( 'NONE',  ( 3.874999999999999556, 3.137999999999999901, -1.320000000000000062 ) ) ;
#3367 = DIRECTION ( 'NONE',  ( -0.7071067811865455743, 8.659560562354955045E-17, -0.7071067811865493491 ) ) ;
#3368 = DIRECTION ( 'NONE',  ( 0.9992912762382413216, 0.03489602031262312859, -0.01411428356268701854 ) ) ;
#3369 = AXIS2_PLACEMENT_3D ( 'NONE', #3280, #7945, #10098 ) ;
#3370 = DIRECTION ( 'NONE',  ( 0.000000000000000000, 0.000000000000000000, -1.000000000000000000 ) ) ;
#3371 = EDGE_CURVE ( 'NONE', #7260, #9538, #4038, .T. ) ;
#3372 = CARTESIAN_POINT ( 'NONE',  ( 3.602264755523620465, 0.9969999999999996643, 0.4491205543005138412 ) ) ;
#3374 = ORIENTED_EDGE ( 'NONE', *, *, #12725, .T. ) ;
#3373 = LINE ( 'NONE', #905, #7244 ) ;
#3375 = ORIENTED_EDGE ( 'NONE', *, *, #7592, .T. ) ;
#3376 = EDGE_CURVE ( 'NONE', #2332, #5034, #839, .T. ) ;
#3377 = CARTESIAN_POINT ( 'NONE',  ( 0.6867356290494768256, 0.03910112949509623320, -0.4280493037418063307 ) ) ;
#3378 = ORIENTED_EDGE ( 'NONE', *, *, #1363, .T. ) ;
#3379 = DIRECTION ( 'NONE',  ( 0.000000000000000000, 0.000000000000000000, -1.000000000000000000 ) ) ;
#3380 = AXIS2_PLACEMENT_3D ( 'NONE', #9510, #10647, #6210 ) ;
#3381 = EDGE_CURVE ( 'NONE', #12094, #8206, #6586, .T. ) ;
#3382 = CARTESIAN_POINT ( 'NONE',  ( 3.046145694169734242, 0.6270559217006406172, -0.4569753433026481071 ) ) ;
#3383 = CARTESIAN_POINT ( 'NONE',  ( 2.322097220813319485, 0.05061516561994754138, 0.4672020166565828414 ) ) ;
#3384 = DIRECTION ( 'NONE',  ( 0.000000000000000000, 1.000000000000000000, 0.000000000000000000 ) ) ;
#3385 = AXIS2_PLACEMENT_3D ( 'NONE', #8219, #6914, #2388 ) ;
#3386 = CIRCLE ( 'NONE', #8289, 3.000000000000000444 ) ;
#3387 = CARTESIAN_POINT ( 'NONE',  ( 0.9743412996626567013, -0.4829530011247266108, -0.3864506351494798597 ) ) ;
#3388 = ORIENTED_EDGE ( 'NONE', *, *, #1011, .F. ) ;
#3389 = AXIS2_PLACEMENT_3D ( 'NONE', #6217, #14314, #11025 ) ;
#3390 = CARTESIAN_POINT ( 'NONE',  ( 3.464667047197554250, 2.040221276569372133, -0.6276463482411095418 ) ) ;
#3391 = FACE_OUTER_BOUND ( 'NONE', #4170, .T. ) ;
#3392 = ORIENTED_EDGE ( 'NONE', *, *, #6259, .F. ) ;
#3393 = CIRCLE ( 'NONE', #13394, 0.1899999999999996136 ) ;
#3394 = LINE ( 'NONE', #10280, #8880 ) ;
#3395 = VERTEX_POINT ( 'NONE', #3709 ) ;
#3396 = DIRECTION ( 'NONE',  ( 0.000000000000000000, 0.000000000000000000, -1.000000000000000000 ) ) ;
#3397 = DIRECTION ( 'NONE',  ( -1.000000000000000000, 0.000000000000000000, 0.000000000000000000 ) ) ;
#3398 = ORIENTED_EDGE ( 'NONE', *, *, #12642, .F. ) ;
#3399 = VECTOR ( 'NONE', #2525, 39.37007874015748143 ) ;
#3400 = CARTESIAN_POINT ( 'NONE',  ( 3.921117472075024146, 1.873018435015763927, -0.4984105334006085908 ) ) ;
#3401 = EDGE_CURVE ( 'NONE', #11384, #3698, #8383, .T. ) ;
#3402 = PRESENTATION_LAYER_ASSIGNMENT (  '', '', ( #13406 ) ) ;
#3403 = CARTESIAN_POINT ( 'NONE',  ( 0.9355712947711312122, -0.4319563074674140912, -0.4615054731933312393 ) ) ;
#3404 = CONICAL_SURFACE ( 'NONE', #11711, 0.2812500000000000555, 0.7853981633974465026 ) ;
#3405 = VECTOR ( 'NONE', #4883, 39.37007874015748143 ) ;
#3406 = CARTESIAN_POINT ( 'NONE',  ( 3.828581658748513306, 1.898678166888137842, 0.4983806998886662343 ) ) ;
#3407 = CARTESIAN_POINT ( 'NONE',  ( 0.7983174577546989781, -0.4829999999999998739, -0.4287183451209413132 ) ) ;
#3408 = VECTOR ( 'NONE', #14961, 39.37007874015748854 ) ;
#3409 = EDGE_LOOP ( 'NONE', ( #12630, #6373, #13508, #1502 ) ) ;
#3410 = ORIENTED_EDGE ( 'NONE', *, *, #958, .T. ) ;
#3411 = AXIS2_PLACEMENT_3D ( 'NONE', #623, #7608, #10981 ) ;
#3412 = CARTESIAN_POINT ( 'NONE',  ( -0.2665675396067773706, 1.593633255602467935, -0.3001969837044509148 ) ) ;
#3413 = ORIENTED_EDGE ( 'NONE', *, *, #4873, .F. ) ;
#3414 = DIRECTION ( 'NONE',  ( 0.000000000000000000, 0.000000000000000000, -1.000000000000000000 ) ) ;
#3415 = DIRECTION ( 'NONE',  ( 0.3420201433256623846, 0.000000000000000000, -0.9396926207859106484 ) ) ;
#3416 = FACE_BOUND ( 'NONE', #1479, .T. ) ;
#3417 = CARTESIAN_POINT ( 'NONE',  ( 0.7006931131589945183, -0.03737057977092374250, -0.4858697363291134552 ) ) ;
#3418 = ORIENTED_EDGE ( 'NONE', *, *, #6233, .F. ) ;
#3419 = EDGE_CURVE ( 'NONE', #12744, #14900, #3977, .T. ) ;
#3420 = CARTESIAN_POINT ( 'NONE',  ( 3.339098075141892163, 2.444574610142927096, -0.5239010158726820077 ) ) ;
#3421 = CARTESIAN_POINT ( 'NONE',  ( 0.6729652567417454545, -0.03979450559140960270, -0.4872362964973816490 ) ) ;
#3422 = DIRECTION ( 'NONE',  ( 0.000000000000000000, 0.000000000000000000, 1.000000000000000000 ) ) ;
#3423 = ORIENTED_EDGE ( 'NONE', *, *, #9805, .T. ) ;
#3425 = ORIENTED_EDGE ( 'NONE', *, *, #1499, .F. ) ;
#3424 = CARTESIAN_POINT ( 'NONE',  ( 0.2577064312470200291, 1.589827634136293355, 0.3155448735949257788 ) ) ;
#3426 = APPLICATION_CONTEXT ( 'automotive_design' ) ;
#3427 = ORIENTED_EDGE ( 'NONE', *, *, #365, .F. ) ;
#3429 = EDGE_LOOP ( 'NONE', ( #3939, #12431, #7108, #8738 ) ) ;
#3428 = DIRECTION ( 'NONE',  ( 0.000000000000000000, 0.000000000000000000, -1.000000000000000000 ) ) ;
#3430 = EDGE_LOOP ( 'NONE', ( #82, #7939, #3111, #10078 ) ) ;
#3431 = ADVANCED_FACE ( 'NONE', ( #5361 ), #2327, .F. ) ;
#3432 = EDGE_CURVE ( 'NONE', #5425, #8382, #10884, .T. ) ;
#3433 = DIRECTION ( 'NONE',  ( 0.000000000000000000, -0.000000000000000000, 1.000000000000000000 ) ) ;
#3434 = PLANE ( 'NONE',  #3058 ) ;
#3435 = EDGE_LOOP ( 'NONE', ( #8390, #3378, #8525, #3718 ) ) ;
#3436 = EDGE_CURVE ( 'NONE', #13119, #8503, #1833, .T. ) ;
#3437 = DIRECTION ( 'NONE',  ( -1.000000000000000000, 0.000000000000000000, 0.000000000000000000 ) ) ;
#3438 = DIRECTION ( 'NONE',  ( -0.000000000000000000, 1.000000000000000000, -0.000000000000000000 ) ) ;
#3439 = CARTESIAN_POINT ( 'NONE',  ( 3.875000000000000000, 0.8660254037844384856, 0.5000000000000002220 ) ) ;
#3440 = CARTESIAN_POINT ( 'NONE',  ( 2.743000000000000327, 1.679378605318042395, -1.679378605318058604 ) ) ;
#3441 = LINE ( 'NONE', #13906, #1783 ) ;
#3442 = EDGE_CURVE ( 'NONE', #1719, #6236, #1895, .T. ) ;
#3443 = CIRCLE ( 'NONE', #8819, 0.1899999999999996136 ) ;
#3444 = CARTESIAN_POINT ( 'NONE',  ( 0.09500000000000431710, -1.679378605318048390, 1.679378605318054163 ) ) ;
#3445 = DIRECTION ( 'NONE',  ( 0.000000000000000000, 0.000000000000000000, -1.000000000000000000 ) ) ;
#3446 = FACE_OUTER_BOUND ( 'NONE', #14295, .T. ) ;
#3447 = LINE ( 'NONE', #15148, #7320 ) ;
#3448 = CARTESIAN_POINT ( 'NONE',  ( 4.531286706020566157, 1.713376479792114049, 0.4628985212650200687 ) ) ;
#3449 = ORIENTED_EDGE ( 'NONE', *, *, #14099, .F. ) ;
#3450 = CARTESIAN_POINT ( 'NONE',  ( 2.807000000000000384, 1.679378605318059048, 1.679378605318041506 ) ) ;
#3452 = ORIENTED_EDGE ( 'NONE', *, *, #12127, .T. ) ;
#3451 = CARTESIAN_POINT ( 'NONE',  ( 3.875000000000000000, 3.567999999999999616, 0.000000000000000000 ) ) ;
#3453 = ORIENTED_EDGE ( 'NONE', *, *, #12031, .T. ) ;
#3454 = CARTESIAN_POINT ( 'NONE',  ( 0.4125000000000000333, 0.000000000000000000, -0.3724999999999999978 ) ) ;
#3455 = ORIENTED_EDGE ( 'NONE', *, *, #9576, .F. ) ;
#3456 = CIRCLE ( 'NONE', #14196, 0.8000000000000000444 ) ;
#3457 = FACE_OUTER_BOUND ( 'NONE', #12822, .T. ) ;
#3458 = CARTESIAN_POINT ( 'NONE',  ( 3.388933043275772050, 0.7513023213622327390, -0.4521337140780258834 ) ) ;
#3459 = DIRECTION ( 'NONE',  ( 1.000000000000000000, 0.000000000000000000, 0.000000000000000000 ) ) ;
#3460 = DIRECTION ( 'NONE',  ( 0.000000000000000000, -1.000000000000000000, 0.000000000000000000 ) ) ;
#3461 = EDGE_CURVE ( 'NONE', #5088, #8576, #1673, .T. ) ;
#3462 = ORIENTED_EDGE ( 'NONE', *, *, #12529, .F. ) ;
#3463 = CARTESIAN_POINT ( 'NONE',  ( 0.6731911676471491468, -0.3979338129854863571, 0.4888638514297523607 ) ) ;
#3464 = CIRCLE ( 'NONE', #4446, 0.2041999999999996596 ) ;
#3465 = CYLINDRICAL_SURFACE ( 'NONE', #9831, 0.06000000000000001860 ) ;
#3466 = DIRECTION ( 'NONE',  ( -1.000000000000000000, 0.000000000000000000, 0.000000000000000000 ) ) ;
#3467 = EDGE_LOOP ( 'NONE', ( #4892, #4858, #8658, #10636 ) ) ;
#3468 = EDGE_CURVE ( 'NONE', #12193, #947, #7645, .T. ) ;
#3469 = DIRECTION ( 'NONE',  ( 0.000000000000000000, 1.000000000000000000, 0.000000000000000000 ) ) ;
#3470 = VERTEX_POINT ( 'NONE', #1813 ) ;
#3471 = DIRECTION ( 'NONE',  ( -1.000000000000000000, -0.000000000000000000, -0.000000000000000000 ) ) ;
#3472 = CARTESIAN_POINT ( 'NONE',  ( 5.546318247523970513, 0.000000000000000000, 0.000000000000000000 ) ) ;
#3473 = ORIENTED_EDGE ( 'NONE', *, *, #6420, .F. ) ;
#3474 = CARTESIAN_POINT ( 'NONE',  ( 3.875000000000000444, 1.884022191776434152, -0.5000000000000002220 ) ) ;
#3475 = AXIS2_PLACEMENT_3D ( 'NONE', #3265, #14968, #11225 ) ;
#3476 = CARTESIAN_POINT ( 'NONE',  ( 2.414213562373088262, 0.1427864376268981050, -0.4064941968476760703 ) ) ;
#3477 = CARTESIAN_POINT ( 'NONE',  ( 2.775039370078740131, -1.679378605318048390, 1.679378605318054163 ) ) ;
#3478 = PLANE ( 'NONE',  #12118 ) ;
#3479 = VECTOR ( 'NONE', #7222, 39.37007874015748854 ) ;
#3480 = EDGE_CURVE ( 'NONE', #11008, #327, #11870, .T. ) ;
#3481 = EDGE_CURVE ( 'NONE', #4487, #12451, #661, .T. ) ;
#3482 = ORIENTED_EDGE ( 'NONE', *, *, #4611, .F. ) ;
#3483 = ORIENTED_EDGE ( 'NONE', *, *, #277, .T. ) ;
#3484 = DIRECTION ( 'NONE',  ( 0.03489949670249522379, -0.9993908270190959842, 0.000000000000000000 ) ) ;
#3485 = ORIENTED_EDGE ( 'NONE', *, *, #3252, .F. ) ;
#3486 = CARTESIAN_POINT ( 'NONE',  ( 2.592367411162173063, 0.4049457270506677808, -0.4633846410852800468 ) ) ;
#3487 = AXIS2_PLACEMENT_3D ( 'NONE', #7031, #12669, #13809 ) ;
#3488 = CARTESIAN_POINT ( 'NONE',  ( 0.9257356467070699813, -0.4653787754209000038, -0.4457641624418894888 ) ) ;
#3489 =( LENGTH_UNIT ( ) NAMED_UNIT ( * ) SI_UNIT ( $, .METRE. ) );
#3490 = CARTESIAN_POINT ( 'NONE',  ( 0.7007544714965479038, -0.04192809431833794537, -0.4875120335496958557 ) ) ;
#3491 = VERTEX_POINT ( 'NONE', #13292 ) ;
#3492 = DIRECTION ( 'NONE',  ( 0.000000000000000000, 0.000000000000000000, -1.000000000000000000 ) ) ;
#3493 = AXIS2_PLACEMENT_3D ( 'NONE', #12111, #1261, #7449 ) ;
#3494 = CARTESIAN_POINT ( 'NONE',  ( 0.6676004498178161883, 0.02173067840223007890, -0.4667915867939429475 ) ) ;
#3495 = DIRECTION ( 'NONE',  ( 0.000000000000000000, 0.000000000000000000, 1.000000000000000000 ) ) ;
#3496 = CARTESIAN_POINT ( 'NONE',  ( 4.685892362381063769, 1.733292669144359976, -0.01737435135451124296 ) ) ;
#3497 = ORIENTED_EDGE ( 'NONE', *, *, #14501, .F. ) ;
#3499 = VERTEX_POINT ( 'NONE', #2833 ) ;
#3498 = CARTESIAN_POINT ( 'NONE',  ( 0.2936128187763883957, 1.600826314462300282, 0.2533531860778008293 ) ) ;
#3500 = ORIENTED_EDGE ( 'NONE', *, *, #12684, .F. ) ;
#3502 = ORIENTED_EDGE ( 'NONE', *, *, #1835, .T. ) ;
#3501 = CARTESIAN_POINT ( 'NONE',  ( 0.8999999999999998002, 0.1549999999999996103, -0.2949999999999999289 ) ) ;
#3503 = ORIENTED_EDGE ( 'NONE', *, *, #6248, .T. ) ;
#3504 = CYLINDRICAL_SURFACE ( 'NONE', #9710, 2.500000000000000000 ) ;
#3505 =( NAMED_UNIT ( * ) SI_UNIT ( $, .STERADIAN. ) SOLID_ANGLE_UNIT ( ) );
#3506 = CARTESIAN_POINT ( 'NONE',  ( 3.875000000000000000, 3.137999999999999901, -0.5000000000000002220 ) ) ;
#3507 = ORIENTED_EDGE ( 'NONE', *, *, #2447, .F. ) ;
#3508 = AXIS2_PLACEMENT_3D ( 'NONE', #9130, #4317, #4394 ) ;
#3509 = CARTESIAN_POINT ( 'NONE',  ( -0.1444440947987238599, 1.589814529920261732, -0.3809527529760087239 ) ) ;
#3510 = CARTESIAN_POINT ( 'NONE',  ( 0.6609607771814278721, -0.4492411629263703410, -0.4835552281312081591 ) ) ;
#3511 = CIRCLE ( 'NONE', #7423, 0.9999999999999996669 ) ;
#3512 = FACE_OUTER_BOUND ( 'NONE', #551, .T. ) ;
#3513 = AXIS2_PLACEMENT_3D ( 'NONE', #2451, #13828, #1212 ) ;
#3514 = DIRECTION ( 'NONE',  ( -1.874307916738609066E-16, 1.000000000000000000, 0.000000000000000000 ) ) ;
#3515 = EDGE_CURVE ( 'NONE', #9898, #11449, #12161, .T. ) ;
#3516 = CARTESIAN_POINT ( 'NONE',  ( 8.792093969802149189, 0.8799778768672790186, 0.1855527009831954288 ) ) ;
#3517 = CARTESIAN_POINT ( 'NONE',  ( 1.375000000000000000, 0.000000000000000000, 0.000000000000000000 ) ) ;
#3518 = EDGE_CURVE ( 'NONE', #13670, #1691, #2581, .T. ) ;
#3519 = DIRECTION ( 'NONE',  ( 0.000000000000000000, 0.7071067811865509034, 0.7071067811865441310 ) ) ;
#3520 = DIRECTION ( 'NONE',  ( -0.9781476007338071321, 2.546183866652743860E-17, -0.2079116908177521816 ) ) ;
#3521 = CARTESIAN_POINT ( 'NONE',  ( 4.374625251963650818, 1.706956914788115842, 0.6219410930580085983 ) ) ;
#3522 = ORIENTED_EDGE ( 'NONE', *, *, #12613, .T. ) ;
#3523 = CARTESIAN_POINT ( 'NONE',  ( 2.774999999999999911, 2.359999999999994547, -1.575000000000016831 ) ) ;
#3525 = VERTEX_POINT ( 'NONE', #4054 ) ;
#3524 = DIRECTION ( 'NONE',  ( 0.000000000000000000, 0.000000000000000000, 1.000000000000000000 ) ) ;
#3526 = ORIENTED_EDGE ( 'NONE', *, *, #3999, .F. ) ;
#3527 = DIRECTION ( 'NONE',  ( 0.000000000000000000, 0.000000000000000000, 1.000000000000000000 ) ) ;
#3528 = EDGE_CURVE ( 'NONE', #14976, #10812, #4538, .T. ) ;
#3529 = CYLINDRICAL_SURFACE ( 'NONE', #4995, 0.3190000000000000058 ) ;
#3530 = ORIENTED_EDGE ( 'NONE', *, *, #1324, .F. ) ;
#3531 = FACE_OUTER_BOUND ( 'NONE', #13889, .T. ) ;
#3532 = AXIS2_PLACEMENT_3D ( 'NONE', #5191, #9855, #6415 ) ;
#3533 = LINE ( 'NONE', #5840, #9420 ) ;
#3534 = EDGE_CURVE ( 'NONE', #8801, #1005, #8459, .T. ) ;
#3535 = LINE ( 'NONE', #11647, #2410 ) ;
#3536 = ORIENTED_EDGE ( 'NONE', *, *, #13859, .F. ) ;
#3537 = EDGE_CURVE ( 'NONE', #6615, #12114, #8036, .T. ) ;
#3538 = CARTESIAN_POINT ( 'NONE',  ( 3.498666114443761188, 1.947009193665356408, -0.6486007100584754159 ) ) ;
#3539 = CARTESIAN_POINT ( 'NONE',  ( 0.5400755080658357077, 0.1749999999999999889, -1.532626322880899838 ) ) ;
#3540 = DIRECTION ( 'NONE',  ( 0.000000000000000000, 0.000000000000000000, 1.000000000000000000 ) ) ;
#3541 = ORIENTED_EDGE ( 'NONE', *, *, #2361, .F. ) ;
#3542 = CARTESIAN_POINT ( 'NONE',  ( 0.2849999999999999756, 4.529999999999999361, 0.4108223460329293864 ) ) ;
#3543 = AXIS2_PLACEMENT_3D ( 'NONE', #13363, #11079, #9725 ) ;
#3544 = CARTESIAN_POINT ( 'NONE',  ( 6.794491571325181667, 1.679378605318059492, 1.679378605318041506 ) ) ;
#3545 = ORIENTED_EDGE ( 'NONE', *, *, #10103, .F. ) ;
#3546 = AXIS2_PLACEMENT_3D ( 'NONE', #7983, #6845, #11499 ) ;
#3547 = AXIS2_PLACEMENT_3D ( 'NONE', #11730, #1375, #8438 ) ;
#3548 = EDGE_CURVE ( 'NONE', #14201, #11113, #5762, .T. ) ;
#3549 = CARTESIAN_POINT ( 'NONE',  ( 2.124999999999999556, 0.000000000000000000, 0.000000000000000000 ) ) ;
#3550 = ORIENTED_EDGE ( 'NONE', *, *, #4611, .T. ) ;
#3551 = EDGE_CURVE ( 'NONE', #11593, #4577, #10176, .T. ) ;
#3552 = CARTESIAN_POINT ( 'NONE',  ( 3.944129661530210385, 1.867491090171841339, -0.4951980309903490363 ) ) ;
#3553 = CARTESIAN_POINT ( 'NONE',  ( 3.426491571325181340, 1.575000000000016387, 2.359999999999999876 ) ) ;
#3554 = ADVANCED_FACE ( 'NONE', ( #4285 ), #13557, .F. ) ;
#3555 = VECTOR ( 'NONE', #8645, 39.37007874015748143 ) ;
#3556 = CARTESIAN_POINT ( 'NONE',  ( 0.06299999999999994493, 1.679378605318035733, -1.679378605318065487 ) ) ;
#3557 = AXIS2_PLACEMENT_3D ( 'NONE', #12, #15020, #7161 ) ;
#3558 = AXIS2_PLACEMENT_3D ( 'NONE', #8128, #2456, #3295 ) ;
#3559 = CARTESIAN_POINT ( 'NONE',  ( 3.739718906115036212, 1.845510024168589558, -0.7378645487154772420 ) ) ;
#3560 = ORIENTED_EDGE ( 'NONE', *, *, #9184, .F. ) ;
#3561 = EDGE_LOOP ( 'NONE', ( #4475, #3905, #2789, #11302 ) ) ;
#3562 = EDGE_CURVE ( 'NONE', #1972, #7174, #9678, .T. ) ;
#3563 = UNCERTAINTY_MEASURE_WITH_UNIT (LENGTH_MEASURE( 1.000000000000000082E-05 ), #4167, 'distance_accuracy_value', 'NONE');
#3564 = CONICAL_SURFACE ( 'NONE', #1351, 0.4070000000000022489, 0.7853981633974547183 ) ;
#3565 = CARTESIAN_POINT ( 'NONE',  ( 3.426491571325181784, 2.015787472269954694, 0.6125935857979679655 ) ) ;
#3566 = ORIENTED_EDGE ( 'NONE', *, *, #13826, .F. ) ;
#3567 = CARTESIAN_POINT ( 'NONE',  ( 0.3390120837646757312, 1.603403006623434379, -0.1747193524918033425 ) ) ;
#3568 = CIRCLE ( 'NONE', #9915, 0.3750000000000004996 ) ;
#3569 = VECTOR ( 'NONE', #12961, 39.37007874015748143 ) ;
#3570 = CARTESIAN_POINT ( 'NONE',  ( 3.874999999999999556, 2.750000000000000000, 1.320000000000000062 ) ) ;
#3571 = DIRECTION ( 'NONE',  ( 1.000000000000000000, 0.000000000000000000, 0.000000000000000000 ) ) ;
#3572 = CARTESIAN_POINT ( 'NONE',  ( -0.4125000000000000333, 0.1859999999999983611, 0.3724999999999999423 ) ) ;
#3573 = ORIENTED_EDGE ( 'NONE', *, *, #13372, .T. ) ;
#3574 = DIRECTION ( 'NONE',  ( 0.000000000000000000, 0.000000000000000000, -1.000000000000000000 ) ) ;
#3575 = EDGE_CURVE ( 'NONE', #10219, #13623, #2207, .T. ) ;
#3576 = CARTESIAN_POINT ( 'NONE',  ( 1.323631913064689192, 7.693249048049262105E-17, 0.4212431828234003972 ) ) ;
#3577 = VECTOR ( 'NONE', #11557, 39.37007874015748143 ) ;
#3578 = CARTESIAN_POINT ( 'NONE',  ( 1.000847373107698779, -0.3829999999999998961, -0.4858637376679703634 ) ) ;
#3579 = CIRCLE ( 'NONE', #12119, 1.999999999999999334 ) ;
#3580 = SURFACE_SIDE_STYLE ('',( #10383 ) ) ;
#3581 = CARTESIAN_POINT ( 'NONE',  ( 4.621558427459308227, 1.809512430825229501, -0.08833967945055898330 ) ) ;
#3582 = ORIENTED_EDGE ( 'NONE', *, *, #13787, .F. ) ;
#3584 = ORIENTED_EDGE ( 'NONE', *, *, #12872, .T. ) ;
#3583 = CARTESIAN_POINT ( 'NONE',  ( 2.743000000000000771, 1.679378605318059048, 1.416878605318041773 ) ) ;
#3585 = VERTEX_POINT ( 'NONE', #11470 ) ;
#3586 = DIRECTION ( 'NONE',  ( 0.000000000000000000, 0.000000000000000000, -1.000000000000000000 ) ) ;
#3587 = EDGE_LOOP ( 'NONE', ( #6462, #7611, #13760, #10593 ) ) ;
#3588 = FACE_BOUND ( 'NONE', #2488, .T. ) ;
#3589 = AXIS2_PLACEMENT_3D ( 'NONE', #7261, #4812, #3428 ) ;
#3590 = DIRECTION ( 'NONE',  ( 0.000000000000000000, 0.000000000000000000, -1.000000000000000000 ) ) ;
#3591 = SHAPE_REPRESENTATION ( 'MAT-052', ( #2049, #14264, #12067, #13510, #11089, #4010, #5476, #4505, #4749, #11331, #13274, #6696, #11833 ), #10859 ) ;
#3592 = ORIENTED_EDGE ( 'NONE', *, *, #2801, .T. ) ;
#3593 = DIRECTION ( 'NONE',  ( 1.000000000000000000, 0.000000000000000000, 0.000000000000000000 ) ) ;
#3594 = CARTESIAN_POINT ( 'NONE',  ( 0.2249147617188449189, 0.7512260236060024354, 0.3723417112827343556 ) ) ;
#3595 = EDGE_CURVE ( 'NONE', #11724, #13670, #9101, .T. ) ;
#3596 = CARTESIAN_POINT ( 'NONE',  ( -0.4124999999999999223, 0.000000000000000000, 0.3724999999999999978 ) ) ;
#3597 = AXIS2_PLACEMENT_3D ( 'NONE', #785, #4260, #12436 ) ;
#3598 = FACE_OUTER_BOUND ( 'NONE', #2803, .T. ) ;
#3599 = PRODUCT_DEFINITION ( 'UNKNOWN', '', #7443, #14727 ) ;
#3600 = CARTESIAN_POINT ( 'NONE',  ( 2.061999999999999389, 0.000000000000000000, 0.000000000000000000 ) ) ;
#3601 = DIRECTION ( 'NONE',  ( 0.000000000000000000, 1.000000000000000000, -0.000000000000000000 ) ) ;
#3602 = CIRCLE ( 'NONE', #10440, 0.4070000000000044138 ) ;
#3603 = DIRECTION ( 'NONE',  ( -1.000000000000000000, -0.000000000000000000, -0.000000000000000000 ) ) ;
#3604 = CARTESIAN_POINT ( 'NONE',  ( 3.426491571325181340, 2.062169880637645836, 0.5999481385559802815 ) ) ;
#3605 = EDGE_LOOP ( 'NONE', ( #14641, #8107, #6723, #13180 ) ) ;
#3606 = FACE_OUTER_BOUND ( 'NONE', #2496, .T. ) ;
#3608 = ORIENTED_EDGE ( 'NONE', *, *, #11734, .F. ) ;
#3607 = FACE_BOUND ( 'NONE', #6697, .T. ) ;
#3609 = VERTEX_POINT ( 'NONE', #3284 ) ;
#3610 = CARTESIAN_POINT ( 'NONE',  ( 0.7100000000000001865, 0.000000000000000000, 0.000000000000000000 ) ) ;
#3611 = CARTESIAN_POINT ( 'NONE',  ( 0.2099999999999999922, 1.559103846021539619, 0.3809527529760087239 ) ) ;
#3612 = DIRECTION ( 'NONE',  ( -1.365923996832131609E-16, 1.000000000000000000, 0.000000000000000000 ) ) ;
#3613 = VERTEX_POINT ( 'NONE', #5662 ) ;
#3614 = DIRECTION ( 'NONE',  ( 0.000000000000000000, 0.000000000000000000, -1.000000000000000000 ) ) ;
#3615 = PRODUCT_DEFINITION ( 'UNKNOWN', '', #14022, #11823 ) ;
#3616 = CARTESIAN_POINT ( 'NONE',  ( -0.4124999999999999223, 0.1749999999999999889, -0.4124999999999999778 ) ) ;
#3617 = DIRECTION ( 'NONE',  ( 0.000000000000000000, 0.000000000000000000, 1.000000000000000000 ) ) ;
#3618 = AXIS2_PLACEMENT_3D ( 'NONE', #7124, #3815, #9565 ) ;
#3619 = ORIENTED_EDGE ( 'NONE', *, *, #7363, .F. ) ;
#3620 = DIRECTION ( 'NONE',  ( 1.000000000000000000, 0.000000000000000000, 0.000000000000000000 ) ) ;
#3621 = CARTESIAN_POINT ( 'NONE',  ( 3.463409033965894945, 1.936472266768732631, -0.7051516699459041693 ) ) ;
#3622 = CARTESIAN_POINT ( 'NONE',  ( 3.426491571325181340, -1.575000000000027489, -2.359999999999989218 ) ) ;
#3623 = CARTESIAN_POINT ( 'NONE',  ( 2.743000000000000771, 1.679378605318059048, 1.679378605318041506 ) ) ;
#3624 = ORIENTED_EDGE ( 'NONE', *, *, #10830, .T. ) ;
#3625 = CARTESIAN_POINT ( 'NONE',  ( 0.4529333289293680509, 0.1749999999999999889, -1.690370196005881009 ) ) ;
#3626 = VERTEX_POINT ( 'NONE', #10320 ) ;
#3627 = VECTOR ( 'NONE', #5777, 39.37007874015748143 ) ;
#3628 = DIRECTION ( 'NONE',  ( 0.000000000000000000, 0.000000000000000000, -1.000000000000000000 ) ) ;
#3629 = ORIENTED_EDGE ( 'NONE', *, *, #9770, .F. ) ;
#3630 = EDGE_CURVE ( 'NONE', #6280, #3743, #5585, .T. ) ;
#3631 = AXIS2_PLACEMENT_3D ( 'NONE', #6499, #10865, #4207 ) ;
#3632 = FACE_OUTER_BOUND ( 'NONE', #12931, .T. ) ;
#3633 = ADVANCED_FACE ( 'NONE', ( #9177 ), #15061, .T. ) ;
#3634 = EDGE_CURVE ( 'NONE', #11355, #10371, #9474, .T. ) ;
#3635 = DIRECTION ( 'NONE',  ( -1.000000000000000000, 0.000000000000000000, 0.000000000000000000 ) ) ;
#3636 = CIRCLE ( 'NONE', #7309, 0.4070000000000055240 ) ;
#3637 = CARTESIAN_POINT ( 'NONE',  ( -0.3725000000000002198, 0.2159999999999999420, -0.4425000000000005596 ) ) ;
#3638 = VECTOR ( 'NONE', #396, 39.37007874015748143 ) ;
#3639 = EDGE_CURVE ( 'NONE', #4204, #7643, #5815, .T. ) ;
#3640 = TOROIDAL_SURFACE ( 'NONE', #3380, 0.5849999999999996314, 0.1000000000000000056 ) ;
#3641 = EDGE_CURVE ( 'NONE', #12635, #11468, #4359, .T. ) ;
#3642 = FACE_OUTER_BOUND ( 'NONE', #8211, .T. ) ;
#3643 = ORIENTED_EDGE ( 'NONE', *, *, #4667, .F. ) ;
#3644 = ORIENTED_EDGE ( 'NONE', *, *, #10305, .T. ) ;
#3645 = CIRCLE ( 'NONE', #12183, 0.3750000000000004996 ) ;
#3646 = VERTEX_POINT ( 'NONE', #14909 ) ;
#3647 = FACE_BOUND ( 'NONE', #15115, .T. ) ;
#3648 = CARTESIAN_POINT ( 'NONE',  ( 0.3117353328467041274, 1.602948811930422712, -0.2219640709471300821 ) ) ;
#3649 = DIRECTION ( 'NONE',  ( 1.000000000000000000, 0.000000000000000000, 0.000000000000000000 ) ) ;
#3650 = AXIS2_PLACEMENT_3D ( 'NONE', #14832, #10401, #14985 ) ;
#3651 = DIRECTION ( 'NONE',  ( -0.000000000000000000, -1.000000000000000000, -0.000000000000000000 ) ) ;
#3652 = ORIENTED_EDGE ( 'NONE', *, *, #11090, .F. ) ;
#3653 = VECTOR ( 'NONE', #9394, 39.37007874015748143 ) ;
#3654 = CARTESIAN_POINT ( 'NONE',  ( 3.874999999999999556, 3.535499999999999421, 1.320000000000000062 ) ) ;
#3655 = CARTESIAN_POINT ( 'NONE',  ( 1.993429504473980929, 0.2774392468042482518, 0.4112782092410766643 ) ) ;
#3656 =( BOUNDED_SURFACE ( )  B_SPLINE_SURFACE ( 3, 2, ( 
 ( #8958, #14759, #4292 ),
 ( #4059, #5439, #10184 ),
 ( #10105, #9954, #6434 ),
 ( #13599, #13680, #4144 ),
 ( #14836, #3146, #8726 ),
 ( #13368, #4367, #9036 ),
 ( #7808, #2048, #1821 ),
 ( #12461, #1977, #6659 ),
 ( #11317, #7579, #13449 ),
 ( #6510, #3215, #6738 ) ),
 .UNSPECIFIED., .F., .F., .F. ) 
 B_SPLINE_SURFACE_WITH_KNOTS ( ( 4, 2, 2, 2, 4 ),
 ( 3, 3 ),
 ( 0.009445390106978779690, 0.01015357746046147147, 0.01086176481394416499, 0.01156995216742685850, 0.01227813952090955202 ),
 ( 0.000000000000000000, 1.000000000000000000 ),
 .UNSPECIFIED. ) 
 GEOMETRIC_REPRESENTATION_ITEM ( )  RATIONAL_B_SPLINE_SURFACE ( (
 ( 1.000000000000000000, 0.7071067811865481278, 1.000000000000000000),
 ( 1.000000000000000000, 0.7078095846774001831, 1.000000000000000000),
 ( 1.000000000000000000, 0.7084372686669646590, 1.000000000000000000),
 ( 1.000000000000000000, 0.7093555124764521214, 1.000000000000000000),
 ( 1.000000000000000000, 0.7096393529300775160, 1.000000000000000000),
 ( 1.000000000000000000, 0.7097449673932565428, 1.000000000000000000),
 ( 1.000000000000000000, 0.7095699935427098870, 1.000000000000000000),
 ( 1.000000000000000000, 0.7088230032924415225, 1.000000000000000000),
 ( 1.000000000000000000, 0.7082619641421786794, 1.000000000000000000),
 ( 1.000000000000000000, 0.7075975758264665405, 1.000000000000000000) ) ) 
 REPRESENTATION_ITEM ( '' )  SURFACE ( )  );
#3657 = DIRECTION ( 'NONE',  ( 0.000000000000000000, 0.000000000000000000, -1.000000000000000000 ) ) ;
#3658 = ADVANCED_FACE ( 'NONE', ( #9032 ), #3138, .T. ) ;
#3659 = AXIS2_PLACEMENT_3D ( 'NONE', #11491, #6910, #11562 ) ;
#3660 = EDGE_CURVE ( 'NONE', #12028, #3309, #1635, .T. ) ;
#3661 = CONICAL_SURFACE ( 'NONE', #688, 0.1520000000000001905, 0.7853981633974460586 ) ;
#3662 = FACE_OUTER_BOUND ( 'NONE', #2322, .T. ) ;
#3663 = CARTESIAN_POINT ( 'NONE',  ( 4.682446348489560428, 1.732706346088367821, -0.07442871938619251282 ) ) ;
#3664 = ORIENTED_EDGE ( 'NONE', *, *, #5910, .T. ) ;
#3666 = ORIENTED_EDGE ( 'NONE', *, *, #6916, .F. ) ;
#3665 = CARTESIAN_POINT ( 'NONE',  ( 0.2405080627748377164, 1.577645543303439313, 0.3453333215960370794 ) ) ;
#3667 = EDGE_CURVE ( 'NONE', #710, #13032, #902, .T. ) ;
#3668 = VERTEX_POINT ( 'NONE', #1126 ) ;
#3669 = DIRECTION ( 'NONE',  ( -0.000000000000000000, -1.000000000000000000, -0.000000000000000000 ) ) ;
#3670 = EDGE_LOOP ( 'NONE', ( #14154, #12414, #5622, #9980 ) ) ;
#3671 = DIRECTION ( 'NONE',  ( 0.000000000000000000, 0.000000000000000000, 1.000000000000000000 ) ) ;
#3672 = APPLICATION_PROTOCOL_DEFINITION ( 'draft international standard', 'automotive_design', 1998, #2936 ) ;
#3673 = DIRECTION ( 'NONE',  ( 0.7071067811865345831, -0.7071067811865603403, 0.000000000000000000 ) ) ;
#3674 = ORIENTED_EDGE ( 'NONE', *, *, #985, .F. ) ;
#3675 = LINE ( 'NONE', #2517, #892 ) ;
#3676 = CARTESIAN_POINT ( 'NONE',  ( 2.774999999999999911, 0.7000000000000026201, 2.400000000000000355 ) ) ;
#3677 = VECTOR ( 'NONE', #3710, 39.37007874015748143 ) ;
#3678 = CYLINDRICAL_SURFACE ( 'NONE', #7112, 0.3750000000000004996 ) ;
#3679 = CARTESIAN_POINT ( 'NONE',  ( 8.477129920625907644, 0.8689790899078102537, 0.3802665265448320064 ) ) ;
#3680 = FACE_OUTER_BOUND ( 'NONE', #10428, .T. ) ;
#3681 = CARTESIAN_POINT ( 'NONE',  ( 0.09035531712817648775, 1.379999999999999671, -0.1564999999999998892 ) ) ;
#3682 = CARTESIAN_POINT ( 'NONE',  ( 4.111704219024688634, 1.727819528799023008, 0.7588929890255357025 ) ) ;
#3683 = EDGE_CURVE ( 'NONE', #14092, #8852, #5813, .T. ) ;
#3684 = EDGE_CURVE ( 'NONE', #13770, #13032, #9490, .T. ) ;
#3685 = SHAPE_REPRESENTATION ( 'Thermostate Flange', ( #8424 ), #12311 ) ;
#3686 = ORIENTED_EDGE ( 'NONE', *, *, #545, .T. ) ;
#3687 = CYLINDRICAL_SURFACE ( 'NONE', #14315, 0.5000000000000000000 ) ;
#3689 = ORIENTED_EDGE ( 'NONE', *, *, #9786, .T. ) ;
#3688 = FACE_OUTER_BOUND ( 'NONE', #6031, .T. ) ;
#3690 = ORIENTED_EDGE ( 'NONE', *, *, #12757, .F. ) ;
#3691 = LINE ( 'NONE', #11792, #13361 ) ;
#3692 = LINE ( 'NONE', #138, #7679 ) ;
#3693 = FACE_OUTER_BOUND ( 'NONE', #1307, .T. ) ;
#3694 = ORIENTED_EDGE ( 'NONE', *, *, #14463, .F. ) ;
#3695 = DIRECTION ( 'NONE',  ( -1.000000000000000000, 0.000000000000000000, -0.000000000000000000 ) ) ;
#3696 = DIRECTION ( 'NONE',  ( 0.000000000000000000, -1.000000000000000000, 0.000000000000000000 ) ) ;
#3697 = LINE ( 'NONE', #3982, #14868 ) ;
#3698 = VERTEX_POINT ( 'NONE', #7193 ) ;
#3699 = CARTESIAN_POINT ( 'NONE',  ( 0.6940259540059589005, -0.4844395603711075249, 0.4146509415068772020 ) ) ;
#3700 = DIRECTION ( 'NONE',  ( 1.000000000000000000, 0.000000000000000000, 0.000000000000000000 ) ) ;
#3701 = CARTESIAN_POINT ( 'NONE',  ( 2.124999999999999556, 1.679378605318059048, 1.679378605318041506 ) ) ;
#3702 = EDGE_LOOP ( 'NONE', ( #1287, #860, #3328, #6038 ) ) ;
#3703 = AXIS2_PLACEMENT_3D ( 'NONE', #3800, #6607, #8895 ) ;
#3704 = CARTESIAN_POINT ( 'NONE',  ( 0.5816197779170538817, 0.1749999999999999889, -1.650520655410200099 ) ) ;
#3705 = EDGE_CURVE ( 'NONE', #8521, #9230, #9412, .T. ) ;
#3706 = VERTEX_POINT ( 'NONE', #6121 ) ;
#3707 = DIRECTION ( 'NONE',  ( -1.000000000000000000, 0.000000000000000000, 0.000000000000000000 ) ) ;
#3708 = ORIENTED_EDGE ( 'NONE', *, *, #15120, .T. ) ;
#3709 = CARTESIAN_POINT ( 'NONE',  ( 3.426491571325181340, 2.058905028113295455, 0.2209981660730358233 ) ) ;
#3710 = DIRECTION ( 'NONE',  ( 0.000000000000000000, -1.000000000000000000, 4.591341165822195764E-16 ) ) ;
#3711 = AXIS2_PLACEMENT_3D ( 'NONE', #14799, #3106, #5171 ) ;
#3712 = LINE ( 'NONE', #11747, #3823 ) ;
#3713 = ADVANCED_FACE ( 'NONE', ( #12831 ), #6542, .F. ) ;
#3714 = ADVANCED_FACE ( 'NONE', ( #13051 ), #163, .T. ) ;
#3715 = ADVANCED_FACE ( 'NONE', ( #12912 ), #13347, .F. ) ;
#3716 = VERTEX_POINT ( 'NONE', #14052 ) ;
#3717 = ORIENTED_EDGE ( 'NONE', *, *, #1824, .T. ) ;
#3718 = ORIENTED_EDGE ( 'NONE', *, *, #8218, .F. ) ;
#3719 = CARTESIAN_POINT ( 'NONE',  ( 3.874999999999999556, 3.567999999999999616, -1.509999999999999787 ) ) ;
#3720 = VECTOR ( 'NONE', #14931, 39.37007874015748143 ) ;
#3721 = CARTESIAN_POINT ( 'NONE',  ( -0.1807106342563527812, 1.379999999999999671, 3.262375646219079751E-17 ) ) ;
#3722 = CARTESIAN_POINT ( 'NONE',  ( 0.9126855013391443894, -0.4618906521135902610, -0.4490017598779234009 ) ) ;
#3723 = EDGE_CURVE ( 'NONE', #8323, #261, #1880, .T. ) ;
#3724 = CARTESIAN_POINT ( 'NONE',  ( 2.774999999999999911, 0.6999999999999599876, -2.400000000000011458 ) ) ;
#3725 = PRODUCT_DEFINITION_SHAPE ( 'NONE', 'NONE',  #15153 ) ;
#3726 = ORIENTED_EDGE ( 'NONE', *, *, #6804, .F. ) ;
#3727 = DIRECTION ( 'NONE',  ( -1.000000000000000000, 0.000000000000000000, 0.000000000000000000 ) ) ;
#3728 = APPLICATION_CONTEXT ( 'automotive_design' ) ;
#3729 = DIRECTION ( 'NONE',  ( 0.000000000000000000, 0.000000000000000000, -1.000000000000000000 ) ) ;
#3730 = DIRECTION ( 'NONE',  ( 0.000000000000000000, 0.000000000000000000, 1.000000000000000000 ) ) ;
#3731 = CARTESIAN_POINT ( 'NONE',  ( -0.3724999999999999423, 0.1749999999999999889, 0.4124999999999999778 ) ) ;
#3732 = ADVANCED_FACE ( 'NONE', ( #8351 ), #2126, .F. ) ;
#3733 = VERTEX_POINT ( 'NONE', #9636 ) ;
#3735 = ORIENTED_EDGE ( 'NONE', *, *, #9316, .T. ) ;
#3734 = LINE ( 'NONE', #1771, #10343 ) ;
#3736 = ORIENTED_EDGE ( 'NONE', *, *, #9164, .F. ) ;
#3737 = CARTESIAN_POINT ( 'NONE',  ( 9.797174393178826150E-17, 0.1749999999999999889, 0.8000000000000000444 ) ) ;
#3738 = ORIENTED_EDGE ( 'NONE', *, *, #725, .T. ) ;
#3739 = AXIS2_PLACEMENT_3D ( 'NONE', #3622, #4925, #8223 ) ;
#3740 = DIRECTION ( 'NONE',  ( 0.000000000000000000, -0.000000000000000000, 1.000000000000000000 ) ) ;
#3741 = DIRECTION ( 'NONE',  ( 1.000000000000000000, 0.000000000000000000, 0.000000000000000000 ) ) ;
#3742 = PLANE ( 'NONE',  #2325 ) ;
#3743 = VERTEX_POINT ( 'NONE', #12983 ) ;
#3744 =( BOUNDED_CURVE ( )  B_SPLINE_CURVE ( 3, ( #6948, #12892, #12970, #103 ),
 .UNSPECIFIED., .F., .F. ) 
 B_SPLINE_CURVE_WITH_KNOTS ( ( 4, 4 ),
 ( 0.7853981633974547183, 1.535889741755017912 ),
 .UNSPECIFIED. ) 
 CURVE ( )  GEOMETRIC_REPRESENTATION_ITEM ( )  RATIONAL_B_SPLINE_CURVE ( ( 1.000000000000000000, 0.9536117119880161974, 0.9536117119880161974, 1.000000000000000000 ) ) 
 REPRESENTATION_ITEM ( '' )  );
#3745 = CARTESIAN_POINT ( 'NONE',  ( 2.774999999999999911, -1.574999999999984190, 1.575000000000033040 ) ) ;
#3746 = DIRECTION ( 'NONE',  ( -0.000000000000000000, -1.000000000000000000, -0.000000000000000000 ) ) ;
#3747 = EDGE_CURVE ( 'NONE', #5710, #11671, #7268, .T. ) ;
#3748 = CARTESIAN_POINT ( 'NONE',  ( 3.855580484743782232, 1.862622002527129617, 0.7500000000000002220 ) ) ;
#3749 = EDGE_CURVE ( 'NONE', #7657, #3626, #10689, .T. ) ;
#3750 = CARTESIAN_POINT ( 'NONE',  ( 2.326828918379971488E-17, 1.159999999999999698, 0.1899999999999999745 ) ) ;
#3751 = FACE_OUTER_BOUND ( 'NONE', #11040, .T. ) ;
#3752 = DIRECTION ( 'NONE',  ( 0.000000000000000000, 0.000000000000000000, 1.000000000000000000 ) ) ;
#3753 = CARTESIAN_POINT ( 'NONE',  ( 3.426491571325181340, -3.360000000000016751, -0.9799999999999434719 ) ) ;
#3754 = EDGE_LOOP ( 'NONE', ( #3973, #5459, #11643, #4358 ) ) ;
#3755 = AXIS2_PLACEMENT_3D ( 'NONE', #5390, #8830, #13470 ) ;
#3756 = CARTESIAN_POINT ( 'NONE',  ( -0.7287617923574205570, 0.2159999999999999420, -0.4425000000000005596 ) ) ;
#3758 = ORIENTED_EDGE ( 'NONE', *, *, #7836, .F. ) ;
#3757 = DIRECTION ( 'NONE',  ( 0.000000000000000000, 1.000000000000000000, 0.000000000000000000 ) ) ;
#3759 = ORIENTED_EDGE ( 'NONE', *, *, #3355, .T. ) ;
#3760 = DIRECTION ( 'NONE',  ( 0.000000000000000000, 1.000000000000000000, 0.000000000000000000 ) ) ;
#3761 = CARTESIAN_POINT ( 'NONE',  ( 2.449076186954514686E-17, -0.4430000000000000049, 0.000000000000000000 ) ) ;
#3762 = EDGE_LOOP ( 'NONE', ( #12427, #7817, #7944, #744 ) ) ;
#3763 = DIRECTION ( 'NONE',  ( 0.000000000000000000, 0.000000000000000000, 1.000000000000000000 ) ) ;
#3764 = EDGE_CURVE ( 'NONE', #6889, #14179, #6780, .T. ) ;
#3765 = EDGE_CURVE ( 'NONE', #8027, #2681, #11777, .T. ) ;
#3766 = CARTESIAN_POINT ( 'NONE',  ( 2.774999999999999911, -2.360000000000000320, 0.9799999999999999822 ) ) ;
#3767 = AXIS2_PLACEMENT_3D ( 'NONE', #12690, #3363, #50 ) ;
#3768 = DIRECTION ( 'NONE',  ( -1.000000000000000000, -0.000000000000000000, -0.000000000000000000 ) ) ;
#3769 = ORIENTED_EDGE ( 'NONE', *, *, #7826, .F. ) ;
#3770 = DIRECTION ( 'NONE',  ( -1.000000000000000000, -0.000000000000000000, -0.000000000000000000 ) ) ;
#3771 = DIRECTION ( 'NONE',  ( 0.000000000000000000, 1.000000000000000000, 0.000000000000000000 ) ) ;
#3772 = CARTESIAN_POINT ( 'NONE',  ( 3.876560711617219379, 2.749999999999999556, 0.000000000000000000 ) ) ;
#3773 = ORIENTED_EDGE ( 'NONE', *, *, #10847, .F. ) ;
#3774 = CARTESIAN_POINT ( 'NONE',  ( 2.774999999999999911, 3.360000000000016751, 0.9799999999999461364 ) ) ;
#3775 = DIRECTION ( 'NONE',  ( -1.000000000000000000, -2.130223169792495565E-16, 0.000000000000000000 ) ) ;
#3776 = ORIENTED_EDGE ( 'NONE', *, *, #10085, .F. ) ;
#3777 = CARTESIAN_POINT ( 'NONE',  ( -0.3480879174158268419, 1.602949672542212989, 0.1589995474869664860 ) ) ;
#3778 = VERTEX_POINT ( 'NONE', #1275 ) ;
#3779 = VECTOR ( 'NONE', #14919, 39.37007874015748143 ) ;
#3780 = CARTESIAN_POINT ( 'NONE',  ( 2.807000000000000828, 1.679378605318042395, -1.416878605318058870 ) ) ;
#3781 = EDGE_CURVE ( 'NONE', #12504, #14976, #10624, .T. ) ;
#3782 = FACE_OUTER_BOUND ( 'NONE', #11353, .T. ) ;
#3783 = ADVANCED_FACE ( 'NONE', ( #15140 ), #7759, .F. ) ;
#3784 = LINE ( 'NONE', #3933, #11198 ) ;
#3785 = AXIS2_PLACEMENT_3D ( 'NONE', #2831, #2979, #5273 ) ;
#3786 = CARTESIAN_POINT ( 'NONE',  ( 3.875000000000000000, 3.085321731235734610, 0.000000000000000000 ) ) ;
#3787 = EDGE_LOOP ( 'NONE', ( #9795, #10789, #13530, #749 ) ) ;
#3788 = ORIENTED_EDGE ( 'NONE', *, *, #10853, .T. ) ;
#3789 = ORIENTED_EDGE ( 'NONE', *, *, #8615, .T. ) ;
#3790 = CARTESIAN_POINT ( 'NONE',  ( 8.476283996537762988, 0.8689495495877206377, -0.3203020658980470503 ) ) ;
#3791 = FACE_OUTER_BOUND ( 'NONE', #13343, .T. ) ;
#3792 = LINE ( 'NONE', #6392, #5672 ) ;
#3793 = AXIS2_PLACEMENT_3D ( 'NONE', #10247, #14907, #2591 ) ;
#3794 = LINE ( 'NONE', #10828, #8294 ) ;
#3795 = CARTESIAN_POINT ( 'NONE',  ( 3.783120606456237045, 1.905778818417516396, -0.4920270134196029210 ) ) ;
#3796 = EDGE_CURVE ( 'NONE', #6889, #8873, #3675, .T. ) ;
#3797 = AXIS2_PLACEMENT_3D ( 'NONE', #12475, #1929, #2152 ) ;
#3798 = VECTOR ( 'NONE', #7068, 39.37007874015748143 ) ;
#3799 = DIRECTION ( 'NONE',  ( -1.000000000000000000, -0.000000000000000000, -0.000000000000000000 ) ) ;
#3800 = CARTESIAN_POINT ( 'NONE',  ( 0.3725000000000000533, 0.1749999999999999889, -0.3724999999999999978 ) ) ;
#3801 = DIRECTION ( 'NONE',  ( 0.000000000000000000, 0.000000000000000000, 1.000000000000000000 ) ) ;
#3802 = AXIS2_PLACEMENT_3D ( 'NONE', #297, #9666, #3775 ) ;
#3803 = ORIENTED_EDGE ( 'NONE', *, *, #6420, .T. ) ;
#3804 = VECTOR ( 'NONE', #7233, 39.37007874015748854 ) ;
#3806 = ORIENTED_EDGE ( 'NONE', *, *, #6528, .F. ) ;
#3805 = DIRECTION ( 'NONE',  ( 0.000000000000000000, 1.000000000000000000, 0.000000000000000000 ) ) ;
#3807 = AXIS2_PLACEMENT_3D ( 'NONE', #12318, #13380, #12466 ) ;
#3808 = ORIENTED_EDGE ( 'NONE', *, *, #4280, .T. ) ;
#3809 = DIRECTION ( 'NONE',  ( -0.000000000000000000, -1.000000000000000000, 0.000000000000000000 ) ) ;
#3810 = VERTEX_POINT ( 'NONE', #14664 ) ;
#3811 = DIRECTION ( 'NONE',  ( 0.000000000000000000, -8.723548215061523903E-15, -1.000000000000000000 ) ) ;
#3812 = SHAPE_DEFINITION_REPRESENTATION ( #6043, #8297 ) ;
#3813 = DIRECTION ( 'NONE',  ( 0.000000000000000000, 0.000000000000000000, -1.000000000000000000 ) ) ;
#3814 = ORIENTED_EDGE ( 'NONE', *, *, #4974, .F. ) ;
#3815 = DIRECTION ( 'NONE',  ( 0.000000000000000000, 1.000000000000000000, -0.000000000000000000 ) ) ;
#3816 = DIRECTION ( 'NONE',  ( 0.000000000000000000, 0.000000000000000000, -1.000000000000000000 ) ) ;
#3817 = EDGE_CURVE ( 'NONE', #9590, #13687, #8565, .T. ) ;
#3818 = EDGE_CURVE ( 'NONE', #7544, #4913, #1150, .T. ) ;
#3819 = AXIS2_PLACEMENT_3D ( 'NONE', #132, #2457, #3524 ) ;
#3820 = CARTESIAN_POINT ( 'NONE',  ( 2.774999999999999911, 1.679378605318042395, -1.384878605318057732 ) ) ;
#3821 = ADVANCED_FACE ( 'NONE', ( #13494 ), #488, .T. ) ;
#3822 = LINE ( 'NONE', #1576, #11581 ) ;
#3823 = VECTOR ( 'NONE', #1244, 39.37007874015748143 ) ;
#3824 = AXIS2_PLACEMENT_3D ( 'NONE', #7017, #11672, #1775 ) ;
#3825 = LINE ( 'NONE', #1579, #8689 ) ;
#3826 = DIRECTION ( 'NONE',  ( 0.000000000000000000, 0.000000000000000000, 1.000000000000000000 ) ) ;
#3827 = ADVANCED_FACE ( 'NONE', ( #9927 ), #9723, .F. ) ;
#3828 = CARTESIAN_POINT ( 'NONE',  ( 3.615813188930276034, 1.869365972618699745, 0.7654627819274841816 ) ) ;
#3829 = DIRECTION ( 'NONE',  ( 0.000000000000000000, 0.7071067811865600072, -0.7071067811865350272 ) ) ;
#3830 = AXIS2_PLACEMENT_3D ( 'NONE', #11236, #13814, #1888 ) ;
#3831 = ORIENTED_EDGE ( 'NONE', *, *, #2931, .T. ) ;
#3832 = DIRECTION ( 'NONE',  ( -1.000000000000000000, -0.000000000000000000, -0.000000000000000000 ) ) ;
#3834 = ORIENTED_EDGE ( 'NONE', *, *, #14195, .F. ) ;
#3833 = CARTESIAN_POINT ( 'NONE',  ( 3.080868217518119678, 0.9969999999999996643, -0.4564849121819474775 ) ) ;
#3835 = ORIENTED_EDGE ( 'NONE', *, *, #9491, .F. ) ;
#3836 = DIRECTION ( 'NONE',  ( -0.9743309173630048114, 0.2251205531944285021, 2.276539994720217179E-15 ) ) ;
#3837 = CARTESIAN_POINT ( 'NONE',  ( 3.046145694169734242, 0.6270559217007690700, 0.4569753433027124445 ) ) ;
#3838 = ORIENTED_EDGE ( 'NONE', *, *, #5518, .T. ) ;
#3839 = CARTESIAN_POINT ( 'NONE',  ( 8.789999999999999147, 0.9969999999999998863, 6.829619984160658046E-17 ) ) ;
#3840 = DIMENSIONAL_EXPONENTS ( 1.000000000000000000, 0.000000000000000000, 0.000000000000000000, 0.000000000000000000, 0.000000000000000000, 0.000000000000000000, 0.000000000000000000 ) ;
#3841 = AXIS2_PLACEMENT_3D ( 'NONE', #13951, #1251, #3414 ) ;
#3842 = CARTESIAN_POINT ( 'NONE',  ( 0.7134904538003040697, 1.075665147505303778E-15, 0.4077598229816906117 ) ) ;
#3843 = LINE ( 'NONE', #1597, #9271 ) ;
#3844 = EDGE_CURVE ( 'NONE', #9226, #9926, #11670, .T. ) ;
#3845 = EDGE_LOOP ( 'NONE', ( #4319, #8287, #5058, #10220, #98, #5618, #9903, #9986, #14760, #3202, #7844, #4895, #6765 ) ) ;
#3846 = CARTESIAN_POINT ( 'NONE',  ( 8.493408712665044769E-17, 0.1956296296296295978, 0.7406097974541305806 ) ) ;
#3847 = VECTOR ( 'NONE', #11058, 39.37007874015748143 ) ;
#3848 = CARTESIAN_POINT ( 'NONE',  ( 0.000000000000000000, 0.000000000000000000, 0.000000000000000000 ) ) ;
#3849 = DIRECTION ( 'NONE',  ( 0.000000000000000000, 0.000000000000000000, -1.000000000000000000 ) ) ;
#3850 = EDGE_CURVE ( 'NONE', #2690, #1229, #10845, .T. ) ;
#3851 = B_SPLINE_CURVE_WITH_KNOTS ( 'NONE', 3,
 ( #3474, #14175, #3400, #3552 ),
 .UNSPECIFIED., .F., .F.,
 ( 4, 4 ),
 ( 0.01431391205243922465, 0.01610857355353898304 ),
 .UNSPECIFIED. ) ;
#3852 = EDGE_LOOP ( 'NONE', ( #4682, #11442, #13630, #1805 ) ) ;
#3853 = DIRECTION ( 'NONE',  ( 0.000000000000000000, 0.000000000000000000, 1.000000000000000000 ) ) ;
#3854 = ORIENTED_EDGE ( 'NONE', *, *, #4089, .F. ) ;
#3855 = EDGE_CURVE ( 'NONE', #10392, #11506, #13605, .T. ) ;
#3856 = VECTOR ( 'NONE', #10600, 39.37007874015748143 ) ;
#3857 = CARTESIAN_POINT ( 'NONE',  ( -0.4274235469976391255, 1.569496918332966784, 0.02158620620080434552 ) ) ;
#3858 = ORIENTED_EDGE ( 'NONE', *, *, #6805, .F. ) ;
#3859 = CARTESIAN_POINT ( 'NONE',  ( 0.7936328852534487721, 0.000000000000000000, -0.1007315414569158740 ) ) ;
#3860 = DIRECTION ( 'NONE',  ( 0.000000000000000000, 0.000000000000000000, -1.000000000000000000 ) ) ;
#3861 = VECTOR ( 'NONE', #8274, 39.37007874015747433 ) ;
#3862 = DIRECTION ( 'NONE',  ( -0.000000000000000000, -0.000000000000000000, -1.000000000000000000 ) ) ;
#3863 = CARTESIAN_POINT ( 'NONE',  ( 1.003096136995459631, -0.4429976034824900655, -0.4258273028168327867 ) ) ;
#3864 = CARTESIAN_POINT ( 'NONE',  ( 0.8999999999999998002, 0.1749999999999999889, -0.4850000000000006528 ) ) ;
#3865 = ORIENTED_EDGE ( 'NONE', *, *, #2333, .T. ) ;
#3866 = ORIENTED_EDGE ( 'NONE', *, *, #5081, .T. ) ;
#3867 = CIRCLE ( 'NONE', #3631, 0.05500000000000146438 ) ;
#3868 = EDGE_LOOP ( 'NONE', ( #3530, #5726, #4984, #10562, #3177 ) ) ;
#3869 = EDGE_CURVE ( 'NONE', #12094, #8646, #2883, .T. ) ;
#3870 = CARTESIAN_POINT ( 'NONE',  ( 0.6180000000000012150, 0.000000000000000000, 3.000000000000000444 ) ) ;
#3871 = LINE ( 'NONE', #9826, #398 ) ;
#3872 = CARTESIAN_POINT ( 'NONE',  ( 0.000000000000000000, 1.109999999999999876, 0.000000000000000000 ) ) ;
#3873 = DIRECTION ( 'NONE',  ( 0.7071067811865460184, 8.659560562354951347E-17, 0.7071067811865490160 ) ) ;
#3874 = AXIS2_PLACEMENT_3D ( 'NONE', #11365, #7854, #14890 ) ;
#3875 = FACE_OUTER_BOUND ( 'NONE', #2827, .T. ) ;
#3876 = CARTESIAN_POINT ( 'NONE',  ( 1.936801488370294866, 0.2309360081137078191, 0.4726440467746176322 ) ) ;
#3877 = CARTESIAN_POINT ( 'NONE',  ( 2.742999999999998995, -1.679378605318059048, -1.679378605318041950 ) ) ;
#3878 = AXIS2_PLACEMENT_3D ( 'NONE', #10125, #10276, #14934 ) ;
#3879 = CONICAL_SURFACE ( 'NONE', #12894, 0.2944999999999998175, 0.7853981633974530530 ) ;
#3880 = AXIS2_PLACEMENT_3D ( 'NONE', #5742, #4515, #10408 ) ;
#3881 = VECTOR ( 'NONE', #14460, 39.37007874015748143 ) ;
#3882 = ORIENTED_EDGE ( 'NONE', *, *, #7195, .F. ) ;
#3883 = ORIENTED_EDGE ( 'NONE', *, *, #3376, .T. ) ;
#3884 = AXIS2_PLACEMENT_3D ( 'NONE', #5337, #7481, #6264 ) ;
#3885 = ORIENTED_EDGE ( 'NONE', *, *, #4468, .F. ) ;
#3886 = LINE ( 'NONE', #14274, #12866 ) ;
#3887 = EDGE_CURVE ( 'NONE', #436, #5452, #10996, .T. ) ;
#3888 = DIRECTION ( 'NONE',  ( -0.3420201433256623846, 0.000000000000000000, 0.9396926207859106484 ) ) ;
#3889 = CARTESIAN_POINT ( 'NONE',  ( 4.307277324112376959, 0.9678925435312534242, 0.2517985120128621856 ) ) ;
#3890 = APPLICATION_PROTOCOL_DEFINITION ( 'draft international standard', 'automotive_design', 1998, #11536 ) ;
#3891 = CYLINDRICAL_SURFACE ( 'NONE', #8680, 0.7849999999999983658 ) ;
#3892 = ORIENTED_EDGE ( 'NONE', *, *, #6160, .T. ) ;
#3893 = CIRCLE ( 'NONE', #12428, 0.03999999999999998002 ) ;
#3894 = DIRECTION ( 'NONE',  ( -1.000000000000000000, -0.000000000000000000, -0.000000000000000000 ) ) ;
#3895 = FACE_OUTER_BOUND ( 'NONE', #6114, .T. ) ;
#3896 = DIRECTION ( 'NONE',  ( 0.000000000000000000, 0.000000000000000000, 1.000000000000000000 ) ) ;
#3897 = CIRCLE ( 'NONE', #10249, 0.4849999999999995981 ) ;
#3898 = AXIS2_PLACEMENT_3D ( 'NONE', #2794, #8614, #6465 ) ;
#3899 = DIRECTION ( 'NONE',  ( 0.000000000000000000, 0.000000000000000000, 1.000000000000000000 ) ) ;
#3900 = CARTESIAN_POINT ( 'NONE',  ( 0.6179999999999965521, 1.679378605318035733, -1.679378605318065487 ) ) ;
#3901 = CARTESIAN_POINT ( 'NONE',  ( 3.790489445559355630, 1.886052406415659410, 0.7452351935336294364 ) ) ;
#3902 = EDGE_CURVE ( 'NONE', #14857, #909, #12360, .T. ) ;
#3903 = LINE ( 'NONE', #3200, #5985 ) ;
#3904 = ADVANCED_FACE ( 'NONE', ( #4033 ), #5044, .T. ) ;
#3905 = ORIENTED_EDGE ( 'NONE', *, *, #12184, .T. ) ;
#3906 = EDGE_CURVE ( 'NONE', #2828, #9755, #8699, .T. ) ;
#3907 = AXIS2_PLACEMENT_3D ( 'NONE', #7065, #8133, #2301 ) ;
#3908 = CARTESIAN_POINT ( 'NONE',  ( 0.6552609544199018421, -0.4103521735780240598, 0.5074720589858902065 ) ) ;
#3910 = ORIENTED_EDGE ( 'NONE', *, *, #2195, .F. ) ;
#3909 = DIRECTION ( 'NONE',  ( -0.000000000000000000, -1.000000000000000000, 0.000000000000000000 ) ) ;
#3911 = ORIENTED_EDGE ( 'NONE', *, *, #793, .T. ) ;
#3912 = CIRCLE ( 'NONE', #10264, 0.1150000000000000050 ) ;
#3913 = DIRECTION ( 'NONE',  ( -0.01412288512831128343, 0.000000000000000000, 0.9999002670844990837 ) ) ;
#3914 = CARTESIAN_POINT ( 'NONE',  ( 0.6552609544199017311, -0.03264782642197579937, -0.5074720589858900954 ) ) ;
#3915 = DIRECTION ( 'NONE',  ( 0.000000000000000000, 1.000000000000000000, 0.000000000000000000 ) ) ;
#3916 = ORIENTED_EDGE ( 'NONE', *, *, #7592, .F. ) ;
#3917 = FACE_OUTER_BOUND ( 'NONE', #14203, .T. ) ;
#3918 = EDGE_CURVE ( 'NONE', #12826, #3132, #2389, .T. ) ;
#3919 = CARTESIAN_POINT ( 'NONE',  ( 0.6729666568098726653, -0.03983805101166792983, 0.4872504569466099000 ) ) ;
#3920 = CARTESIAN_POINT ( 'NONE',  ( 0.09500000000000431710, 1.679378605318035733, -2.054378605318066153 ) ) ;
#3921 = AXIS2_PLACEMENT_3D ( 'NONE', #12754, #2283, #6966 ) ;
#3922 = VERTEX_POINT ( 'NONE', #11063 ) ;
#3923 = CARTESIAN_POINT ( 'NONE',  ( 3.394491571325180423, -1.679378605318059048, -1.416878605318056872 ) ) ;
#3924 = DIRECTION ( 'NONE',  ( -0.000000000000000000, -1.000000000000000000, -0.000000000000000000 ) ) ;
#3925 = CARTESIAN_POINT ( 'NONE',  ( 2.372215031318393841, 0.1847933472068912786, -0.4664941379757289175 ) ) ;
#3926 = ORIENTED_EDGE ( 'NONE', *, *, #11203, .T. ) ;
#3927 = DIRECTION ( 'NONE',  ( -0.000000000000000000, -1.000000000000000000, -0.000000000000000000 ) ) ;
#3928 = VERTEX_POINT ( 'NONE', #12212 ) ;
#3929 = ORIENTED_EDGE ( 'NONE', *, *, #1084, .F. ) ;
#3930 = CARTESIAN_POINT ( 'NONE',  ( 6.176491571325181340, -1.679378605318048390, 1.679378605318054163 ) ) ;
#3931 = EDGE_CURVE ( 'NONE', #7544, #6090, #13344, .T. ) ;
#3932 = FACE_OUTER_BOUND ( 'NONE', #2143, .T. ) ;
#3933 = CARTESIAN_POINT ( 'NONE',  ( 3.426491571325181340, -2.359999999999979892, 1.575000000000016387 ) ) ;
#3934 = EDGE_CURVE ( 'NONE', #7832, #5232, #5119, .T. ) ;
#3935 = PLANE ( 'NONE',  #333 ) ;
#3936 = VECTOR ( 'NONE', #15118, 39.37007874015748143 ) ;
#3937 = CARTESIAN_POINT ( 'NONE',  ( 3.394491571325180423, -1.679378605318059048, -1.416878605318056872 ) ) ;
#3938 = DIMENSIONAL_EXPONENTS ( 1.000000000000000000, 0.000000000000000000, 0.000000000000000000, 0.000000000000000000, 0.000000000000000000, 0.000000000000000000, 0.000000000000000000 ) ;
#3939 = ORIENTED_EDGE ( 'NONE', *, *, #2706, .T. ) ;
#3940 = ORIENTED_EDGE ( 'NONE', *, *, #13641, .T. ) ;
#3941 = ORIENTED_EDGE ( 'NONE', *, *, #12214, .T. ) ;
#3942 = DIRECTION ( 'NONE',  ( 0.000000000000000000, 0.000000000000000000, -1.000000000000000000 ) ) ;
#3943 = CYLINDRICAL_SURFACE ( 'NONE', #4578, 0.9999999999999996669 ) ;
#3944 = CARTESIAN_POINT ( 'NONE',  ( 3.875000000000000000, 3.170499999999999208, -0.4849999999999995981 ) ) ;
#3945 = DIRECTION ( 'NONE',  ( 0.000000000000000000, 0.000000000000000000, -1.000000000000000000 ) ) ;
#3946 = CIRCLE ( 'NONE', #13941, 0.5000000000000001110 ) ;
#3947 = LINE ( 'NONE', #13328, #15124 ) ;
#3948 = DIRECTION ( 'NONE',  ( -0.000000000000000000, -1.000000000000000000, -0.000000000000000000 ) ) ;
#3949 = EDGE_CURVE ( 'NONE', #2400, #909, #2959, .T. ) ;
#3950 = EDGE_CURVE ( 'NONE', #2859, #1313, #7552, .T. ) ;
#3951 = CIRCLE ( 'NONE', #14697, 0.1249999999999999861 ) ;
#3952 = ORIENTED_EDGE ( 'NONE', *, *, #895, .F. ) ;
#3953 = EDGE_LOOP ( 'NONE', ( #6954, #13050, #5351, #3500 ) ) ;
#3954 = VERTEX_POINT ( 'NONE', #559 ) ;
#3955 = CARTESIAN_POINT ( 'NONE',  ( 0.04538567959942203800, 1.602419810250338861, 0.3809527529760087239 ) ) ;
#3956 = DIRECTION ( 'NONE',  ( 0.000000000000000000, 0.000000000000000000, -1.000000000000000000 ) ) ;
#3957 = CARTESIAN_POINT ( 'NONE',  ( 3.891549542033483355, 0.8660254037844384856, 0.5000000000000000000 ) ) ;
#3958 = SHAPE_DEFINITION_REPRESENTATION ( #271, #1014 ) ;
#3959 = PLANE ( 'NONE',  #7773 ) ;
#3960 = ORIENTED_EDGE ( 'NONE', *, *, #14017, .T. ) ;
#3961 = CARTESIAN_POINT ( 'NONE',  ( -0.6412116890856959239, -0.6590000000000000302, 0.000000000000000000 ) ) ;
#3962 = CARTESIAN_POINT ( 'NONE',  ( -0.7500000000000001110, 1.000000000000000222, -1.000000000000000000 ) ) ;
#3963 = CARTESIAN_POINT ( 'NONE',  ( 0.09500000000000431710, 1.679378605318059492, 2.054378605318042172 ) ) ;
#3964 = FACE_OUTER_BOUND ( 'NONE', #4912, .T. ) ;
#3965 = DIRECTION ( 'NONE',  ( 0.000000000000000000, 0.000000000000000000, -1.000000000000000000 ) ) ;
#3966 = CARTESIAN_POINT ( 'NONE',  ( 3.414300654442014693, 1.988601236139950545, 0.5922175483633206339 ) ) ;
#3967 = CARTESIAN_POINT ( 'NONE',  ( -0.3724999999999999423, 0.1749999999999999889, -0.3724999999999999978 ) ) ;
#3968 = AXIS2_PLACEMENT_3D ( 'NONE', #2766, #3986, #8444 ) ;
#3969 = ORIENTED_EDGE ( 'NONE', *, *, #468, .T. ) ;
#3970 = DIRECTION ( 'NONE',  ( 0.000000000000000000, 0.000000000000000000, 1.000000000000000000 ) ) ;
#3972 = ORIENTED_EDGE ( 'NONE', *, *, #4898, .T. ) ;
#3971 = FACE_BOUND ( 'NONE', #9914, .T. ) ;
#3973 = ORIENTED_EDGE ( 'NONE', *, *, #9098, .F. ) ;
#3974 = FACE_OUTER_BOUND ( 'NONE', #411, .T. ) ;
#3975 = CARTESIAN_POINT ( 'NONE',  ( 8.849999999999999645, 0.9399413264884247665, 0.2203075555454639400 ) ) ;
#3976 = ORIENTED_EDGE ( 'NONE', *, *, #5112, .T. ) ;
#3977 = LINE ( 'NONE', #9867, #15036 ) ;
#3978 = DIRECTION ( 'NONE',  ( 0.000000000000000000, 0.7071067811865392461, 0.7071067811865555663 ) ) ;
#3979 = AXIS2_PLACEMENT_3D ( 'NONE', #32, #3268, #2109 ) ;
#3980 = ADVANCED_FACE ( 'NONE', ( #5253 ), #13426, .F. ) ;
#3981 = CARTESIAN_POINT ( 'NONE',  ( 0.6766092641689648302, -0.01690956365765576563, 0.4729901586420273696 ) ) ;
#3982 = CARTESIAN_POINT ( 'NONE',  ( -0.7287617923574203349, -0.6590000000000000302, 0.4424999999999983391 ) ) ;
#3983 = ORIENTED_EDGE ( 'NONE', *, *, #12144, .F. ) ;
#3984 = DIRECTION ( 'NONE',  ( -0.000000000000000000, -1.000000000000000000, -0.000000000000000000 ) ) ;
#3985 = AXIS2_PLACEMENT_3D ( 'NONE', #4200, #6797, #10020 ) ;
#3986 = DIRECTION ( 'NONE',  ( -1.000000000000000000, -0.000000000000000000, -0.000000000000000000 ) ) ;
#3987 = FILL_AREA_STYLE_COLOUR ( '', #2419 ) ;
#3988 = ORIENTED_EDGE ( 'NONE', *, *, #8778, .F. ) ;
#3989 = EDGE_CURVE ( 'NONE', #7401, #4697, #5415, .T. ) ;
#3990 = DIRECTION ( 'NONE',  ( -1.000000000000000000, -0.000000000000000000, -0.000000000000000000 ) ) ;
#3991 = VERTEX_POINT ( 'NONE', #1874 ) ;
#3992 = CARTESIAN_POINT ( 'NONE',  ( -0.2667400994511678891, 1.593697031032158318, 0.2998981012866184237 ) ) ;
#3993 = ORIENTED_EDGE ( 'NONE', *, *, #5124, .F. ) ;
#3994 = DIRECTION ( 'NONE',  ( 0.000000000000000000, -1.000000000000000000, 0.000000000000000000 ) ) ;
#3995 = CYLINDRICAL_SURFACE ( 'NONE', #704, 0.1899999999999996136 ) ;
#3996 = EDGE_CURVE ( 'NONE', #9577, #11355, #2134, .T. ) ;
#3997 = CIRCLE ( 'NONE', #11323, 0.5000000000000000000 ) ;
#3998 = CARTESIAN_POINT ( 'NONE',  ( 0.8259541526021394464, -0.4394713480196544286, -0.3620748417912383887 ) ) ;
#3999 = EDGE_CURVE ( 'NONE', #1865, #5661, #10079, .T. ) ;
#4000 = CYLINDRICAL_SURFACE ( 'NONE', #12171, 0.1249999999999999029 ) ;
#4001 = CARTESIAN_POINT ( 'NONE',  ( 6.176491571325181340, -1.679378605318047946, -1.679378605318053497 ) ) ;
#4002 = B_SPLINE_CURVE_WITH_KNOTS ( 'NONE', 3,
 ( #7961, #2052, #10262, #4444, #2989, #9110, #6741, #8811, #11399, #747, #1826, #3218, #5516, #13452 ),
 .UNSPECIFIED., .F., .F.,
 ( 4, 2, 2, 2, 2, 2, 4 ),
 ( 0.001800564375689165265, 0.003589287776566951402, 0.005378011177444737105, 0.008955457979200349278, 0.01253290478095596232, 0.01432162818183375236, 0.01611035158271154066 ),
 .UNSPECIFIED. ) ;
#4003 = CARTESIAN_POINT ( 'NONE',  ( 1.748545107151228573, 0.1138129195078436268, -0.4149214987681278943 ) ) ;
#4004 = EDGE_CURVE ( 'NONE', #4107, #4727, #4757, .T. ) ;
#4005 = AXIS2_PLACEMENT_3D ( 'NONE', #9273, #11718, #9499 ) ;
#4006 = ORIENTED_EDGE ( 'NONE', *, *, #1363, .F. ) ;
#4007 = VERTEX_POINT ( 'NONE', #6136 ) ;
#4008 = ORIENTED_EDGE ( 'NONE', *, *, #9987, .F. ) ;
#4009 = EDGE_CURVE ( 'NONE', #3169, #9348, #5826, .T. ) ;
#4010 = AXIS2_PLACEMENT_3D ( 'NONE', #2120, #5958, #10547 ) ;
#4011 = CARTESIAN_POINT ( 'NONE',  ( 8.803302564019885423, 0.8803692896022989878, -0.1890918720381968565 ) ) ;
#4012 = DIRECTION ( 'NONE',  ( 0.7071067811865436870, 0.000000000000000000, -0.7071067811865512365 ) ) ;
#4013 = DIRECTION ( 'NONE',  ( -1.000000000000000000, 0.000000000000000000, 1.224646799147353207E-16 ) ) ;
#4014 = LINE ( 'NONE', #10980, #3638 ) ;
#4015 = DIRECTION ( 'NONE',  ( 1.000000000000000000, 0.000000000000000000, 0.000000000000000000 ) ) ;
#4016 = CARTESIAN_POINT ( 'NONE',  ( 4.247253441970699761, 1.781917319165590818, 0.6538529083206351400 ) ) ;
#4017 = VECTOR ( 'NONE', #3829, 39.37007874015748143 ) ;
#4018 = VERTEX_POINT ( 'NONE', #11866 ) ;
#4019 = CARTESIAN_POINT ( 'NONE',  ( 2.774999999999999911, 1.679378605318059048, 1.384878605318042855 ) ) ;
#4020 = EDGE_CURVE ( 'NONE', #4756, #13120, #9651, .T. ) ;
#4021 = VERTEX_POINT ( 'NONE', #9429 ) ;
#4022 = ORIENTED_EDGE ( 'NONE', *, *, #8339, .T. ) ;
#4023 = VECTOR ( 'NONE', #12558, 39.37007874015748143 ) ;
#4024 = ORIENTED_EDGE ( 'NONE', *, *, #2219, .F. ) ;
#4025 = CARTESIAN_POINT ( 'NONE',  ( 2.742999999999998995, -1.679378605318059048, -1.416878605318056872 ) ) ;
#4026 = AXIS2_PLACEMENT_3D ( 'NONE', #5014, #8745, #7520 ) ;
#4027 = VECTOR ( 'NONE', #11334, 39.37007874015748143 ) ;
#4028 = DIRECTION ( 'NONE',  ( 0.000000000000000000, 0.000000000000000000, 1.000000000000000000 ) ) ;
#4029 = CARTESIAN_POINT ( 'NONE',  ( 4.368325430995946945, 0.9966752972897022778, 0.08311465223410480219 ) ) ;
#4030 = EDGE_CURVE ( 'NONE', #4777, #6416, #2871, .T. ) ;
#4031 = DIRECTION ( 'NONE',  ( -0.4999999999999918954, 0.000000000000000000, 0.8660254037844431485 ) ) ;
#4032 = ORIENTED_EDGE ( 'NONE', *, *, #11368, .T. ) ;
#4033 = FACE_OUTER_BOUND ( 'NONE', #2033, .T. ) ;
#4034 = CARTESIAN_POINT ( 'NONE',  ( 3.874999999999999556, 2.782000000000000917, -1.320000000000000062 ) ) ;
#4035 = CARTESIAN_POINT ( 'NONE',  ( 0.06299999999999994493, 0.000000000000000000, 0.000000000000000000 ) ) ;
#4036 = AXIS2_PLACEMENT_3D ( 'NONE', #8349, #12909, #3813 ) ;
#4037 = CARTESIAN_POINT ( 'NONE',  ( 8.664307099992964112, 0.9344797629247902915, 0.3304588241376503199 ) ) ;
#4038 = CIRCLE ( 'NONE', #6489, 0.3803340137431718282 ) ;
#4039 = AXIS2_PLACEMENT_3D ( 'NONE', #10265, #4447, #11485 ) ;
#4040 = DIRECTION ( 'NONE',  ( 0.000000000000000000, 0.000000000000000000, -1.000000000000000000 ) ) ;
#4041 = FACE_OUTER_BOUND ( 'NONE', #521, .T. ) ;
#4043 = ORIENTED_EDGE ( 'NONE', *, *, #11946, .F. ) ;
#4042 = LINE ( 'NONE', #8707, #10129 ) ;
#4044 = ORIENTED_EDGE ( 'NONE', *, *, #9331, .T. ) ;
#4045 = CARTESIAN_POINT ( 'NONE',  ( 3.426491571325181784, 2.000448480535557128, 0.6224710308823616645 ) ) ;
#4047 = ORIENTED_EDGE ( 'NONE', *, *, #545, .F. ) ;
#4046 = DIRECTION ( 'NONE',  ( 0.000000000000000000, 0.000000000000000000, -1.000000000000000000 ) ) ;
#4048 = EDGE_LOOP ( 'NONE', ( #7440, #12276, #5163, #3020 ) ) ;
#4049 = DIRECTION ( 'NONE',  ( 0.000000000000000000, 1.000000000000000000, -0.000000000000000000 ) ) ;
#4050 = EDGE_CURVE ( 'NONE', #2101, #5835, #4914, .T. ) ;
#4051 =( NAMED_UNIT ( * ) PLANE_ANGLE_UNIT ( ) SI_UNIT ( $, .RADIAN. ) );
#4052 = CARTESIAN_POINT ( 'NONE',  ( 3.426491571325181340, -0.9799999999999986500, -3.359999999999999876 ) ) ;
#4053 = EDGE_LOOP ( 'NONE', ( #14189, #4242, #2664, #1832 ) ) ;
#4054 = CARTESIAN_POINT ( 'NONE',  ( -0.3724999999999999423, 0.1749999999999999889, -0.4124999999999999778 ) ) ;
#4055 = PLANE ( 'NONE',  #14622 ) ;
#4056 = CIRCLE ( 'NONE', #12848, 0.2499999999999999167 ) ;
#4057 = AXIS2_PLACEMENT_3D ( 'NONE', #5165, #9825, #6461 ) ;
#4058 = DIRECTION ( 'NONE',  ( 0.000000000000000000, 0.000000000000000000, 1.000000000000000000 ) ) ;
#4059 = CARTESIAN_POINT ( 'NONE',  ( 1.004564342297052937, -0.4429999999999998939, -0.3264090227193217064 ) ) ;
#4060 = ORIENTED_EDGE ( 'NONE', *, *, #9917, .T. ) ;
#4061 = VECTOR ( 'NONE', #6977, 39.37007874015748143 ) ;
#4062 = DIRECTION ( 'NONE',  ( 0.000000000000000000, 0.000000000000000000, -1.000000000000000000 ) ) ;
#4063 = CARTESIAN_POINT ( 'NONE',  ( 2.774999999999999911, 1.679378605318042395, -1.679378605318058604 ) ) ;
#4064 =( LENGTH_UNIT ( ) NAMED_UNIT ( * ) SI_UNIT ( $, .METRE. ) );
#4065 = VECTOR ( 'NONE', #12483, 39.37007874015748143 ) ;
#4066 = CARTESIAN_POINT ( 'NONE',  ( 4.140646859253616974, 0.9057630807910989068, -0.4238992791336257393 ) ) ;
#4067 = FACE_OUTER_BOUND ( 'NONE', #952, .T. ) ;
#4068 = ORIENTED_EDGE ( 'NONE', *, *, #14567, .F. ) ;
#4069 = CARTESIAN_POINT ( 'NONE',  ( -0.2285544654201572545, 1.564824237736550439, 0.3660375595475592325 ) ) ;
#4070 = VERTEX_POINT ( 'NONE', #12999 ) ;
#4071 = LINE ( 'NONE', #12250, #6585 ) ;
#4072 = AXIS2_PLACEMENT_3D ( 'NONE', #7186, #14046, #3586 ) ;
#4073 = CARTESIAN_POINT ( 'NONE',  ( 2.633946444925666874, 0.3625193201794745801, -0.4033906250602101173 ) ) ;
#4074 = CARTESIAN_POINT ( 'NONE',  ( 1.552356239822777484, 3.287267395616053572E-16, -0.4178403161916763864 ) ) ;
#4075 = CARTESIAN_POINT ( 'NONE',  ( 1.254789639631331388, -0.3704945895121533050, 0.4822769824910828618 ) ) ;
#4076 = CARTESIAN_POINT ( 'NONE',  ( 0.8318304347846213753, -0.4310575137535593848, -0.3436027928218019500 ) ) ;
#4077 = DIRECTION ( 'NONE',  ( 0.000000000000000000, 0.000000000000000000, -1.000000000000000000 ) ) ;
#4078 = CARTESIAN_POINT ( 'NONE',  ( 0.000000000000000000, 1.379999999999999671, 0.000000000000000000 ) ) ;
#4079 = DIRECTION ( 'NONE',  ( 0.7071067811865512365, 8.659560562354884787E-17, 0.7071067811865436870 ) ) ;
#4080 = AXIS2_PLACEMENT_3D ( 'NONE', #9769, #3809, #14426 ) ;
#4081 = LINE ( 'NONE', #8749, #7895 ) ;
#4082 = ORIENTED_EDGE ( 'NONE', *, *, #11770, .F. ) ;
#4083 = ORIENTED_EDGE ( 'NONE', *, *, #255, .T. ) ;
#4084 = ADVANCED_FACE ( 'NONE', ( #6056 ), #10948, .F. ) ;
#4085 = ORIENTED_EDGE ( 'NONE', *, *, #13997, .T. ) ;
#4086 = EDGE_CURVE ( 'NONE', #12132, #9328, #4598, .T. ) ;
#4087 = CARTESIAN_POINT ( 'NONE',  ( 8.840280274186273601, 0.9396554517976997145, -0.09865722066565443815 ) ) ;
#4088 = VERTEX_POINT ( 'NONE', #11726 ) ;
#4089 = EDGE_CURVE ( 'NONE', #14900, #13770, #14298, .T. ) ;
#4090 = DIRECTION ( 'NONE',  ( 0.000000000000000000, -1.000000000000000000, 9.641816448226552334E-15 ) ) ;
#4091 = AXIS2_PLACEMENT_3D ( 'NONE', #3745, #3593, #9487 ) ;
#4092 = CARTESIAN_POINT ( 'NONE',  ( 0.007386697474241961034, -0.2214999999999999469, -0.5229781811763313248 ) ) ;
#4093 = DIRECTION ( 'NONE',  ( -1.000000000000000000, 0.000000000000000000, 0.000000000000000000 ) ) ;
#4094 = EDGE_CURVE ( 'NONE', #1606, #9348, #8431, .T. ) ;
#4095 = ADVANCED_FACE ( 'NONE', ( #214 ), #11428, .F. ) ;
#4096 = CARTESIAN_POINT ( 'NONE',  ( 4.559113081901449149, 1.797916179321159769, 0.3118124478677711808 ) ) ;
#4097 = CIRCLE ( 'NONE', #9522, 1.000000000000000222 ) ;
#4098 = CARTESIAN_POINT ( 'NONE',  ( 2.743000000000000327, 1.679378605318042395, -1.416878605318059314 ) ) ;
#4099 = AXIS2_PLACEMENT_3D ( 'NONE', #13288, #1519, #4131 ) ;
#4100 = VERTEX_POINT ( 'NONE', #2534 ) ;
#4101 = VERTEX_POINT ( 'NONE', #9582 ) ;
#4102 = ORIENTED_EDGE ( 'NONE', *, *, #10637, .T. ) ;
#4103 = CARTESIAN_POINT ( 'NONE',  ( 0.03632416821535690982, 1.602793162442987418, 0.3809527529760087794 ) ) ;
#4104 = LINE ( 'NONE', #6403, #3847 ) ;
#4105 = CARTESIAN_POINT ( 'NONE',  ( 4.307237825407486120, 0.9678748784477505529, -0.2518665318215109195 ) ) ;
#4106 = CARTESIAN_POINT ( 'NONE',  ( 2.977166378292719351, 0.8979166429007084949, 0.4579496274252440879 ) ) ;
#4107 = VERTEX_POINT ( 'NONE', #2612 ) ;
#4108 = CARTESIAN_POINT ( 'NONE',  ( -0.4124999999999999223, 0.1749999999999999889, -0.4124999999999999778 ) ) ;
#4109 = CARTESIAN_POINT ( 'NONE',  ( 3.875000000000000000, 3.137999999999999901, -0.5000000000000002220 ) ) ;
#4110 = LINE ( 'NONE', #1650, #7080 ) ;
#4111 = CIRCLE ( 'NONE', #7308, 3.000000000000000444 ) ;
#4112 = CIRCLE ( 'NONE', #15104, 0.2041999999999996596 ) ;
#4113 = EDGE_CURVE ( 'NONE', #5284, #6726, #9159, .T. ) ;
#4114 = B_SPLINE_CURVE_WITH_KNOTS ( 'NONE', 3,
 ( #6782, #10295, #11358, #7634, #13357, #11441, #571, #2898, #5267, #4412, #14885, #1806, #12296, #7565, #6421, #3412, #4481, #14957, #9939, #12226, #9150, #14594 ),
 .UNSPECIFIED., .F., .F.,
 ( 4, 2, 2, 2, 2, 2, 2, 2, 2, 2, 4 ),
 ( 2.884201068394857235E-07, 0.0006930185370347780819, 0.001385748653962716676, 0.002771208887818601887, 0.004156669121674489049, 0.005542129355530375778, 0.006927589589386263375, 0.008313049823242149236, 0.009698510057098036832, 0.01039124017402597716, 0.01108397029095391749 ),
 .UNSPECIFIED. ) ;
#4115 = AXIS2_PLACEMENT_3D ( 'NONE', #12735, #2260, #4644 ) ;
#4116 = CARTESIAN_POINT ( 'NONE',  ( 8.705855184453634266, 0.9357017671275056347, 0.3021636316006244272 ) ) ;
#4117 = DIRECTION ( 'NONE',  ( -1.000000000000000000, 0.000000000000000000, 0.000000000000000000 ) ) ;
#4118 = VECTOR ( 'NONE', #1594, 39.37007874015748854 ) ;
#4119 = CYLINDRICAL_SURFACE ( 'NONE', #2004, 1.000000000000000000 ) ;
#4120 = EDGE_CURVE ( 'NONE', #8206, #5828, #8282, .T. ) ;
#4121 = CARTESIAN_POINT ( 'NONE',  ( 4.306829794387749821, 1.729417409056954291, 0.6145795567947273108 ) ) ;
#4123 = ORIENTED_EDGE ( 'NONE', *, *, #10034, .F. ) ;
#4122 = CARTESIAN_POINT ( 'NONE',  ( -0.3725000000000002198, 0.1859999999999983611, -0.4125000000000000333 ) ) ;
#4124 = ORIENTED_EDGE ( 'NONE', *, *, #13636, .T. ) ;
#4125 = CARTESIAN_POINT ( 'NONE',  ( 2.124999999999999556, -1.679378605318059048, -1.679378605318041950 ) ) ;
#4127 = ORIENTED_EDGE ( 'NONE', *, *, #12315, .F. ) ;
#4126 = LINE ( 'NONE', #8640, #7006 ) ;
#4128 = AXIS2_PLACEMENT_3D ( 'NONE', #12385, #5283, #6589 ) ;
#4129 = ORIENTED_EDGE ( 'NONE', *, *, #14591, .T. ) ;
#4130 = AXIS2_PLACEMENT_3D ( 'NONE', #9732, #14458, #6215 ) ;
#4131 = DIRECTION ( 'NONE',  ( 0.000000000000000000, 0.000000000000000000, -1.000000000000000000 ) ) ;
#4132 =( LENGTH_UNIT ( ) NAMED_UNIT ( * ) SI_UNIT ( $, .METRE. ) );
#4133 = CYLINDRICAL_SURFACE ( 'NONE', #4513, 0.7849999999999993650 ) ;
#4134 = VERTEX_POINT ( 'NONE', #4987 ) ;
#4135 = AXIS2_PLACEMENT_3D ( 'NONE', #5074, #12734, #4416 ) ;
#4136 = CARTESIAN_POINT ( 'NONE',  ( 0.06299999999999994493, -1.679378605318048390, 1.679378605318054163 ) ) ;
#4137 = DIRECTION ( 'NONE',  ( -1.000000000000000000, 0.000000000000000000, 0.000000000000000000 ) ) ;
#4138 = CIRCLE ( 'NONE', #10002, 2.500000000000000000 ) ;
#4139 = LINE ( 'NONE', #11084, #2796 ) ;
#4140 = CIRCLE ( 'NONE', #202, 0.8083085967350902568 ) ;
#4141 = DIMENSIONAL_EXPONENTS ( 1.000000000000000000, 0.000000000000000000, 0.000000000000000000, 0.000000000000000000, 0.000000000000000000, 0.000000000000000000, 0.000000000000000000 ) ;
#4142 = CARTESIAN_POINT ( 'NONE',  ( 0.7007173259569011714, -0.03973197056396925858, 0.4867265490097323344 ) ) ;
#4143 =( BOUNDED_CURVE ( )  B_SPLINE_CURVE ( 3, ( #8600, #528, #4074, #7516 ),
 .UNSPECIFIED., .F., .F. ) 
 B_SPLINE_CURVE_WITH_KNOTS ( ( 4, 4 ),
 ( 3.926990816987240063, 4.712388980384689674 ),
 .UNSPECIFIED. ) 
 CURVE ( )  GEOMETRIC_REPRESENTATION_ITEM ( )  RATIONAL_B_SPLINE_CURVE ( ( 1.000000000000000000, 0.9492530216741910110, 0.9492530216741910110, 1.000000000000000000 ) ) 
 REPRESENTATION_ITEM ( '' )  );
#4144 = CARTESIAN_POINT ( 'NONE',  ( 0.9738596046707562737, -0.4829585099714701069, -0.3606225395865768069 ) ) ;
#4145 = EDGE_CURVE ( 'NONE', #2489, #13460, #4846, .T. ) ;
#4146 = ORIENTED_EDGE ( 'NONE', *, *, #5910, .F. ) ;
#4147 = ADVANCED_FACE ( 'NONE', ( #136 ), #8741, .F. ) ;
#4148 = CIRCLE ( 'NONE', #13159, 2.500000000000000000 ) ;
#4149 = CARTESIAN_POINT ( 'NONE',  ( 2.774999999999999911, 1.679378605318059048, 1.679378605318041506 ) ) ;
#4150 = CARTESIAN_POINT ( 'NONE',  ( 6.787121492585022509, 1.224646799147353207E-16, -1.000000000000000000 ) ) ;
#4151 =( NAMED_UNIT ( * ) SI_UNIT ( $, .STERADIAN. ) SOLID_ANGLE_UNIT ( ) );
#4152 = ORIENTED_EDGE ( 'NONE', *, *, #11852, .F. ) ;
#4153 = DIRECTION ( 'NONE',  ( 0.7071067811865523467, 0.000000000000000000, -0.7071067811865425767 ) ) ;
#4154 = DIRECTION ( 'NONE',  ( 0.000000000000000000, 0.000000000000000000, 1.000000000000000000 ) ) ;
#4155 = ORIENTED_EDGE ( 'NONE', *, *, #12989, .F. ) ;
#4156 = DIRECTION ( 'NONE',  ( -1.000000000000000000, -0.000000000000000000, -0.000000000000000000 ) ) ;
#4157 = ORIENTED_EDGE ( 'NONE', *, *, #14933, .F. ) ;
#4158 =( NAMED_UNIT ( * ) PLANE_ANGLE_UNIT ( ) SI_UNIT ( $, .RADIAN. ) );
#4159 = DIRECTION ( 'NONE',  ( -3.491481338843132961E-15, 0.000000000000000000, 1.000000000000000000 ) ) ;
#4160 = CIRCLE ( 'NONE', #5382, 0.2944999999999987073 ) ;
#4161 = CARTESIAN_POINT ( 'NONE',  ( 0.8418300605894717403, -0.4429999999999996163, -0.3276580719765712635 ) ) ;
#4162 = CARTESIAN_POINT ( 'NONE',  ( 3.268630585053793405E-17, -0.5030000000000000027, 0.000000000000000000 ) ) ;
#4163 = ORIENTED_EDGE ( 'NONE', *, *, #5961, .F. ) ;
#4164 = DIRECTION ( 'NONE',  ( -0.000000000000000000, -1.000000000000000000, -0.000000000000000000 ) ) ;
#4165 = EDGE_CURVE ( 'NONE', #8481, #9027, #3691, .T. ) ;
#4166 = DIRECTION ( 'NONE',  ( -1.000000000000000000, -0.000000000000000000, -0.000000000000000000 ) ) ;
#4167 =( CONVERSION_BASED_UNIT ( 'INCH', #5228 ) LENGTH_UNIT ( ) NAMED_UNIT ( #1768 ) );
#4168 = DIRECTION ( 'NONE',  ( 0.000000000000000000, -0.7071067811865600072, -0.7071067811865350272 ) ) ;
#4169 = VERTEX_POINT ( 'NONE', #2687 ) ;
#4170 = EDGE_LOOP ( 'NONE', ( #13287, #9721, #2751, #1462 ) ) ;
#4171 = ORIENTED_EDGE ( 'NONE', *, *, #13515, .F. ) ;
#4172 = DIRECTION ( 'NONE',  ( 0.000000000000000000, 0.000000000000000000, 1.000000000000000000 ) ) ;
#4173 = ORIENTED_EDGE ( 'NONE', *, *, #4094, .T. ) ;
#4174 = DIRECTION ( 'NONE',  ( -0.7071067811865557884, 0.000000000000000000, 0.7071067811865392461 ) ) ;
#4175 = DIRECTION ( 'NONE',  ( 0.000000000000000000, 1.000000000000000000, -0.000000000000000000 ) ) ;
#4176 = DIRECTION ( 'NONE',  ( 0.7071067811865471286, 8.659560562354939021E-17, 0.7071067811865479058 ) ) ;
#4177 = CARTESIAN_POINT ( 'NONE',  ( 4.512342262853154651, 1.791038700169719444, 0.3986247651315083518 ) ) ;
#4178 = EDGE_CURVE ( 'NONE', #9328, #12926, #1221, .T. ) ;
#4179 = ORIENTED_EDGE ( 'NONE', *, *, #4555, .T. ) ;
#4180 = EDGE_CURVE ( 'NONE', #2273, #13657, #9543, .T. ) ;
#4181 = VERTEX_POINT ( 'NONE', #10567 ) ;
#4182 = VERTEX_POINT ( 'NONE', #7497 ) ;
#4183 = EDGE_CURVE ( 'NONE', #7356, #524, #5135, .T. ) ;
#4184 = EDGE_LOOP ( 'NONE', ( #4434, #2987, #5808, #7121 ) ) ;
#4185 = FACE_OUTER_BOUND ( 'NONE', #10949, .T. ) ;
#4186 = LINE ( 'NONE', #7697, #7029 ) ;
#4187 = CARTESIAN_POINT ( 'NONE',  ( 0.09500000000000431710, 1.679378605318035733, -1.304378605318064821 ) ) ;
#4188 = CARTESIAN_POINT ( 'NONE',  ( -0.09067304051454433411, 1.599165379501958695, 0.3809527529760087239 ) ) ;
#4189 = ORIENTED_EDGE ( 'NONE', *, *, #940, .F. ) ;
#4190 = CARTESIAN_POINT ( 'NONE',  ( 2.527624975756972425, 3.137999999999999901, -0.9199802545633498640 ) ) ;
#4191 = CARTESIAN_POINT ( 'NONE',  ( 3.874999999999999556, 2.782000000000002693, 1.320000000000000062 ) ) ;
#4192 = CARTESIAN_POINT ( 'NONE',  ( 2.088768908813758873, 0.2870784642939425146, -0.4704976142822915319 ) ) ;
#4193 = LINE ( 'NONE', #12364, #2714 ) ;
#4194 = ADVANCED_FACE ( 'NONE', ( #3051, #12080 ), #12230, .T. ) ;
#4195 = EDGE_CURVE ( 'NONE', #9577, #184, #10909, .T. ) ;
#4196 = VECTOR ( 'NONE', #5396, 39.37007874015748143 ) ;
#4197 = LINE ( 'NONE', #8860, #1844 ) ;
#4198 = CARTESIAN_POINT ( 'NONE',  ( 0.9483256016623491380, -0.4339531631712009174, -0.4584628122268601946 ) ) ;
#4199 = CARTESIAN_POINT ( 'NONE',  ( 4.245121452821247310, 1.732603396039932520, 0.6542235875937751910 ) ) ;
#4201 = VERTEX_POINT ( 'NONE', #7640 ) ;
#4200 = CARTESIAN_POINT ( 'NONE',  ( 2.806999999999999496, -1.679378605318041950, 1.679378605318059048 ) ) ;
#4202 = ORIENTED_EDGE ( 'NONE', *, *, #144, .F. ) ;
#4204 = VERTEX_POINT ( 'NONE', #14599 ) ;
#4203 = CARTESIAN_POINT ( 'NONE',  ( 0.000000000000000000, 2.258248697627719244E-16, 1.812500000000000222 ) ) ;
#4205 = ORIENTED_EDGE ( 'NONE', *, *, #1738, .T. ) ;
#4206 = ADVANCED_FACE ( 'NONE', ( #9864 ), #8644, .F. ) ;
#4207 = DIRECTION ( 'NONE',  ( 1.000000000000000000, 0.000000000000000000, 0.000000000000000000 ) ) ;
#4208 = SHAPE_REPRESENTATION_RELATIONSHIP ( 'NONE' , 'NONE' ,  #3685, #12215 ) ;
#4209 = DIRECTION ( 'NONE',  ( 0.01412288512831583534, 0.000000000000000000, 0.9999002670844989726 ) ) ;
#4210 = VERTEX_POINT ( 'NONE', #10027 ) ;
#4211 = AXIS2_PLACEMENT_3D ( 'NONE', #6099, #10827, #10761 ) ;
#4212 = CARTESIAN_POINT ( 'NONE',  ( 2.774999999999999911, 0.000000000000000000, 0.000000000000000000 ) ) ;
#4213 = PLANE ( 'NONE',  #8296 ) ;
#4214 = EDGE_CURVE ( 'NONE', #13739, #6474, #14598, .T. ) ;
#4215 = CARTESIAN_POINT ( 'NONE',  ( 2.381437798646418358, 0.6472152511677208286, -0.4058409478271036708 ) ) ;
#4216 = LINE ( 'NONE', #14526, #442 ) ;
#4217 = ORIENTED_EDGE ( 'NONE', *, *, #9417, .T. ) ;
#4218 = CARTESIAN_POINT ( 'NONE',  ( 0.1900000000000001132, -1.002374524060224757E-18, 0.000000000000000000 ) ) ;
#4219 = CARTESIAN_POINT ( 'NONE',  ( 3.378341036178184265, 0.9983173952992376865, -0.06652291956437350606 ) ) ;
#4220 = CARTESIAN_POINT ( 'NONE',  ( 3.944129661530210385, 1.761538328845252188, -0.7935532608319411096 ) ) ;
#4221 = EDGE_CURVE ( 'NONE', #803, #9092, #8515, .T. ) ;
#4222 = ORIENTED_EDGE ( 'NONE', *, *, #14850, .T. ) ;
#4223 = CARTESIAN_POINT ( 'NONE',  ( 0.7020471549603384265, -0.4140285412429734468, 0.4816513823572639574 ) ) ;
#4224 = DIRECTION ( 'NONE',  ( 0.000000000000000000, 0.000000000000000000, 1.000000000000000000 ) ) ;
#4225 = EDGE_LOOP ( 'NONE', ( #8061, #4656 ) ) ;
#4226 = DIRECTION ( 'NONE',  ( 0.000000000000000000, 0.000000000000000000, 1.000000000000000000 ) ) ;
#4227 = EDGE_LOOP ( 'NONE', ( #537, #2772, #12825, #13403 ) ) ;
#4228 = AXIS2_PLACEMENT_3D ( 'NONE', #6216, #14391, #9662 ) ;
#4229 = ADVANCED_FACE ( 'NONE', ( #12158 ), #8799, .F. ) ;
#4230 = ADVANCED_FACE ( 'NONE', ( #3974 ), #13441, .F. ) ;
#4231 = FACE_OUTER_BOUND ( 'NONE', #7636, .T. ) ;
#4232 =( BOUNDED_CURVE ( )  B_SPLINE_CURVE ( 3, ( #12441, #6638, #10155, #14813 ),
 .UNSPECIFIED., .F., .F. ) 
 B_SPLINE_CURVE_WITH_KNOTS ( ( 4, 4 ),
 ( 1.605702911834775870, 2.356194490192339064 ),
 .UNSPECIFIED. ) 
 CURVE ( )  GEOMETRIC_REPRESENTATION_ITEM ( )  RATIONAL_B_SPLINE_CURVE ( ( 1.000000000000000000, 0.9536117119880161974, 0.9536117119880161974, 1.000000000000000000 ) ) 
 REPRESENTATION_ITEM ( '' )  );
#4233 = CARTESIAN_POINT ( 'NONE',  ( 0.000000000000000000, 1.249999999999999778, -0.2812500000000000555 ) ) ;
#4234 = CYLINDRICAL_SURFACE ( 'NONE', #3703, 0.03999999999999998002 ) ;
#4235 = DIRECTION ( 'NONE',  ( 0.000000000000000000, 0.000000000000000000, -1.000000000000000000 ) ) ;
#4236 = CARTESIAN_POINT ( 'NONE',  ( 0.000000000000000000, 1.836970198721030181E-16, -1.500000000000000222 ) ) ;
#4237 = ORIENTED_EDGE ( 'NONE', *, *, #1765, .F. ) ;
#4238 = CARTESIAN_POINT ( 'NONE',  ( 1.564978703518703496, 0.1749999999999999889, -0.4193347797797316034 ) ) ;
#4239 = CARTESIAN_POINT ( 'NONE',  ( 3.897807165016460740, 1.773345575131051621, 0.7975644729706475866 ) ) ;
#4240 = CARTESIAN_POINT ( 'NONE',  ( 0.06299999999999994493, 1.679378605318035733, -1.679378605318065487 ) ) ;
#4241 = EDGE_LOOP ( 'NONE', ( #12709, #6054 ) ) ;
#4242 = ORIENTED_EDGE ( 'NONE', *, *, #12833, .F. ) ;
#4243 = ORIENTED_EDGE ( 'NONE', *, *, #805, .F. ) ;
#4244 = CONICAL_SURFACE ( 'NONE', #59, 0.2624999999999852451, 0.7853981633974423948 ) ;
#4245 = CARTESIAN_POINT ( 'NONE',  ( 2.774999999999999911, 0.000000000000000000, 0.000000000000000000 ) ) ;
#4246 = CONICAL_SURFACE ( 'NONE', #12777, 0.3750000000000007772, 0.7853981633974536081 ) ;
#4247 = CARTESIAN_POINT ( 'NONE',  ( 0.6821548861275755771, -0.4360442393940396344, -0.4605830663053250285 ) ) ;
#4248 = EDGE_CURVE ( 'NONE', #10100, #1606, #3867, .T. ) ;
#4249 = LINE ( 'NONE', #11430, #451 ) ;
#4250 = CARTESIAN_POINT ( 'NONE',  ( 4.616842326592714763, 1.808536722254569629, -0.1228515035735000954 ) ) ;
#4251 = ORIENTED_EDGE ( 'NONE', *, *, #885, .F. ) ;
#4252 = FACE_OUTER_BOUND ( 'NONE', #4617, .T. ) ;
#4253 = VECTOR ( 'NONE', #11493, 39.37007874015748143 ) ;
#4254 = AXIS2_PLACEMENT_3D ( 'NONE', #12851, #8291, #65 ) ;
#4255 = CARTESIAN_POINT ( 'NONE',  ( 4.201664376791202749, 1.786179860254142104, -0.6761149289075030211 ) ) ;
#4256 = ORIENTED_EDGE ( 'NONE', *, *, #6062, .F. ) ;
#4257 = ORIENTED_EDGE ( 'NONE', *, *, #3667, .F. ) ;
#4258 = ORIENTED_EDGE ( 'NONE', *, *, #889, .F. ) ;
#4259 = CARTESIAN_POINT ( 'NONE',  ( 0.2846118995245459082, 1.599166939805951593, -0.2689432355368134853 ) ) ;
#4260 = DIRECTION ( 'NONE',  ( 1.365923996832131609E-16, -1.000000000000000000, -0.000000000000000000 ) ) ;
#4261 = CARTESIAN_POINT ( 'NONE',  ( 3.426491571325181340, -0.6999999999999587663, 2.400000000000012790 ) ) ;
#4262 = CARTESIAN_POINT ( 'NONE',  ( -0.1787546228633429546, 1.577672892097735646, 0.3809527529760086129 ) ) ;
#4263 = VERTEX_POINT ( 'NONE', #11157 ) ;
#4264 = CIRCLE ( 'NONE', #12796, 0.4349999999999999423 ) ;
#4265 = DIRECTION ( 'NONE',  ( 0.000000000000000000, 1.000000000000000000, 0.000000000000000000 ) ) ;
#4266 = LINE ( 'NONE', #2884, #7078 ) ;
#4267 = DIRECTION ( 'NONE',  ( 0.7071067811865452413, 8.659560562354961208E-17, 0.7071067811865497932 ) ) ;
#4268 = CARTESIAN_POINT ( 'NONE',  ( 8.474190026735612946, 0.9969999999999998863, -0.3203020658980470503 ) ) ;
#4269 = CARTESIAN_POINT ( 'NONE',  ( 8.635695252271263556, 0.8745163133035790404, 0.2783269381325281788 ) ) ;
#4270 = CARTESIAN_POINT ( 'NONE',  ( 0.9652705920801475381, -0.4828330467331340969, -0.4119425203458967344 ) ) ;
#4271 = CARTESIAN_POINT ( 'NONE',  ( 4.212694554283068271, 1.735282967767267426, 0.6714771266614066869 ) ) ;
#4272 = VECTOR ( 'NONE', #11891, 39.37007874015748143 ) ;
#4274 = ORIENTED_EDGE ( 'NONE', *, *, #3551, .F. ) ;
#4273 = DIRECTION ( 'NONE',  ( 0.000000000000000000, -0.000000000000000000, 1.000000000000000000 ) ) ;
#4275 = AXIS2_PLACEMENT_3D ( 'NONE', #1990, #3384, #2068 ) ;
#4276 = ORIENTED_EDGE ( 'NONE', *, *, #706, .T. ) ;
#4278 = ORIENTED_EDGE ( 'NONE', *, *, #13418, .F. ) ;
#4277 = FACE_BOUND ( 'NONE', #6079, .T. ) ;
#4279 = ORIENTED_EDGE ( 'NONE', *, *, #696, .T. ) ;
#4280 = EDGE_CURVE ( 'NONE', #15092, #5075, #6064, .T. ) ;
#4281 = ADVANCED_FACE ( 'NONE', ( #13216 ), #12401, .T. ) ;
#4282 = FACE_BOUND ( 'NONE', #3297, .T. ) ;
#4283 = ORIENTED_EDGE ( 'NONE', *, *, #11591, .T. ) ;
#4284 = EDGE_CURVE ( 'NONE', #6179, #1969, #14978, .T. ) ;
#4285 = FACE_OUTER_BOUND ( 'NONE', #11578, .T. ) ;
#4286 = CARTESIAN_POINT ( 'NONE',  ( -0.4125000000000001998, 0.1859999999999983611, -0.4125000000000000333 ) ) ;
#4287 = AXIS2_PLACEMENT_3D ( 'NONE', #5582, #12521, #8033 ) ;
#4288 = AXIS2_PLACEMENT_3D ( 'NONE', #890, #12686, #1973 ) ;
#4289 = AXIS2_PLACEMENT_3D ( 'NONE', #2295, #5746, #4600 ) ;
#4290 = EDGE_CURVE ( 'NONE', #6222, #4182, #6794, .T. ) ;
#4291 = CARTESIAN_POINT ( 'NONE',  ( 3.601417382415922130, 1.056999999999999718, -0.3891265382754439117 ) ) ;
#4292 = CARTESIAN_POINT ( 'NONE',  ( 0.9652173913043479159, -0.4829999999999998739, -0.3379636412230419551 ) ) ;
#4293 = ORIENTED_EDGE ( 'NONE', *, *, #14542, .F. ) ;
#4294 = DIRECTION ( 'NONE',  ( 0.000000000000000000, 0.000000000000000000, -1.000000000000000000 ) ) ;
#4295 = LINE ( 'NONE', #6514, #11048 ) ;
#4296 = CARTESIAN_POINT ( 'NONE',  ( 3.851998792340888933, 1.785879153954030851, -0.7996516825436228437 ) ) ;
#4297 = ORIENTED_EDGE ( 'NONE', *, *, #6342, .F. ) ;
#4298 = CARTESIAN_POINT ( 'NONE',  ( 3.941974925529625473, 0.8684515238967140949, -0.4957779064694355919 ) ) ;
#4299 = CARTESIAN_POINT ( 'NONE',  ( 0.4125000000000000333, 0.1749999999999999889, -0.4124999999999999778 ) ) ;
#4300 = ORIENTED_EDGE ( 'NONE', *, *, #11529, .F. ) ;
#4301 = AXIS2_PLACEMENT_3D ( 'NONE', #13499, #8934, #9932 ) ;
#4302 = AXIS2_PLACEMENT_3D ( 'NONE', #2416, #9464, #8329 ) ;
#4303 = FACE_OUTER_BOUND ( 'NONE', #9580, .T. ) ;
#4304 = SURFACE_SIDE_STYLE ('',( #2999 ) ) ;
#4305 = LINE ( 'NONE', #8192, #10026 ) ;
#4306 = AXIS2_PLACEMENT_3D ( 'NONE', #7283, #3757, #13522 ) ;
#4307 = CARTESIAN_POINT ( 'NONE',  ( 2.774999999999999911, -0.6999999999999989564, -2.399999999999999911 ) ) ;
#4308 = DIRECTION ( 'NONE',  ( 0.000000000000000000, 0.000000000000000000, -1.000000000000000000 ) ) ;
#4309 = FACE_OUTER_BOUND ( 'NONE', #2630, .T. ) ;
#4310 = AXIS2_PLACEMENT_3D ( 'NONE', #12069, #272, #10851 ) ;
#4311 = EDGE_CURVE ( 'NONE', #8521, #7375, #8017, .T. ) ;
#4312 = AXIS2_PLACEMENT_3D ( 'NONE', #10208, #4321, #4398 ) ;
#4313 = VERTEX_POINT ( 'NONE', #5580 ) ;
#4314 = DIRECTION ( 'NONE',  ( -1.000000000000000000, -0.000000000000000000, -0.000000000000000000 ) ) ;
#4315 = CARTESIAN_POINT ( 'NONE',  ( 3.426491571325181340, 1.954234464180151676, 0.6847610993685215863 ) ) ;
#4316 = EDGE_CURVE ( 'NONE', #2489, #8413, #10704, .T. ) ;
#4317 = DIRECTION ( 'NONE',  ( 1.000000000000000000, 0.000000000000000000, 0.000000000000000000 ) ) ;
#4318 = VERTEX_POINT ( 'NONE', #12453 ) ;
#4319 = ORIENTED_EDGE ( 'NONE', *, *, #12895, .T. ) ;
#4320 = AXIS2_PLACEMENT_3D ( 'NONE', #2750, #572, #5427 ) ;
#4321 = DIRECTION ( 'NONE',  ( -0.000000000000000000, -1.000000000000000000, -0.000000000000000000 ) ) ;
#4322 = ORIENTED_EDGE ( 'NONE', *, *, #9251, .F. ) ;
#4323 = LINE ( 'NONE', #3178, #5240 ) ;
#4324 = CARTESIAN_POINT ( 'NONE',  ( 0.6601485485260571995, -0.3723516483516484121, -0.5137583810202325241 ) ) ;
#4325 = CARTESIAN_POINT ( 'NONE',  ( 2.774999999999999911, 1.679378605318042395, -1.973878605318059698 ) ) ;
#4326 = DIRECTION ( 'NONE',  ( 0.000000000000000000, 0.000000000000000000, 1.000000000000000000 ) ) ;
#4327 = CIRCLE ( 'NONE', #625, 0.5000000000000002220 ) ;
#4328 = ORIENTED_EDGE ( 'NONE', *, *, #8650, .T. ) ;
#4329 = ADVANCED_FACE ( 'NONE', ( #4583 ), #3135, .F. ) ;
#4330 = VECTOR ( 'NONE', #6785, 39.37007874015748854 ) ;
#4331 = VERTEX_POINT ( 'NONE', #13673 ) ;
#4332 = VERTEX_POINT ( 'NONE', #12597 ) ;
#4333 = UNCERTAINTY_MEASURE_WITH_UNIT (LENGTH_MEASURE( 1.000000000000000082E-05 ), #14625, 'distance_accuracy_value', 'NONE');
#4334 = ORIENTED_EDGE ( 'NONE', *, *, #7082, .F. ) ;
#4335 = CARTESIAN_POINT ( 'NONE',  ( 2.774999999999999911, -2.359999999999984333, 1.575000000000016387 ) ) ;
#4336 = DIRECTION ( 'NONE',  ( 0.000000000000000000, 0.000000000000000000, -1.000000000000000000 ) ) ;
#4337 = CYLINDRICAL_SURFACE ( 'NONE', #10747, 0.08500000000000004774 ) ;
#4338 = CONTEXT_DEPENDENT_SHAPE_REPRESENTATION ( #5281, #8493 ) ;
#4339 = PLANE ( 'NONE',  #11443 ) ;
#4340 = ORIENTED_EDGE ( 'NONE', *, *, #4346, .T. ) ;
#4341 = CARTESIAN_POINT ( 'NONE',  ( 3.134971565885993794, 2.497487542101918923, -0.1157722030434289312 ) ) ;
#4342 = CARTESIAN_POINT ( 'NONE',  ( 1.003096136995459631, -0.4429976034824900655, -0.4258273028168327867 ) ) ;
#4343 = DIRECTION ( 'NONE',  ( -0.9992912762382415437, -0.03489602031261518356, 0.01411428356269074126 ) ) ;
#4344 = AXIS2_PLACEMENT_3D ( 'NONE', #14581, #14355, #1647 ) ;
#4345 = CARTESIAN_POINT ( 'NONE',  ( 0.9740510491226479495, -0.4388824337986295676, -0.4485312320239642769 ) ) ;
#4346 = EDGE_CURVE ( 'NONE', #10024, #4007, #10317, .T. ) ;
#4347 = CARTESIAN_POINT ( 'NONE',  ( 4.336468708500340163, 1.779575802716562016, 0.5927141824020646377 ) ) ;
#4349 = EDGE_LOOP ( 'NONE', ( #12450, #245, #130, #4624 ) ) ;
#4348 = DIRECTION ( 'NONE',  ( -0.000000000000000000, -1.000000000000000000, -0.000000000000000000 ) ) ;
#4350 = AXIS2_PLACEMENT_3D ( 'NONE', #10590, #9535, #2483 ) ;
#4351 = ORIENTED_EDGE ( 'NONE', *, *, #2265, .T. ) ;
#4353 = ORIENTED_EDGE ( 'NONE', *, *, #2556, .T. ) ;
#4352 = FACE_BOUND ( 'NONE', #2975, .T. ) ;
#4354 = ORIENTED_EDGE ( 'NONE', *, *, #7650, .F. ) ;
#4355 = AXIS2_PLACEMENT_3D ( 'NONE', #14905, #1970, #5658 ) ;
#4356 = CARTESIAN_POINT ( 'NONE',  ( 0.000000000000000000, 1.239999999999999991, 0.000000000000000000 ) ) ;
#4357 = FACE_OUTER_BOUND ( 'NONE', #1493, .T. ) ;
#4358 = ORIENTED_EDGE ( 'NONE', *, *, #6925, .F. ) ;
#4359 = LINE ( 'NONE', #1045, #10939 ) ;
#4360 = CARTESIAN_POINT ( 'NONE',  ( 0.6653056208004449745, -0.4594276363813551423, -0.4725671546919800181 ) ) ;
#4361 = CIRCLE ( 'NONE', #6814, 0.3750000000000004996 ) ;
#4362 = AXIS2_PLACEMENT_3D ( 'NONE', #10905, #7395, #1627 ) ;
#4363 = LINE ( 'NONE', #12604, #14261 ) ;
#4364 = AXIS2_PLACEMENT_3D ( 'NONE', #8581, #6138, #3763 ) ;
#4365 = CARTESIAN_POINT ( 'NONE',  ( 2.774999999999999911, 0.000000000000000000, 0.000000000000000000 ) ) ;
#4366 = ADVANCED_FACE ( 'NONE', ( #3206, #14752, #2119, #13817, #4282, #10246 ), #13590, .T. ) ;
#4367 = CARTESIAN_POINT ( 'NONE',  ( 0.9751458587006417433, -0.4432411459049188096, -0.3788907315698128997 ) ) ;
#4368 = ADVANCED_FACE ( 'NONE', ( #13740 ), #2038, .T. ) ;
#4369 = EDGE_LOOP ( 'NONE', ( #2614, #7241, #13987, #7799 ) ) ;
#4370 = EDGE_CURVE ( 'NONE', #3613, #14462, #11466, .T. ) ;
#4371 = CARTESIAN_POINT ( 'NONE',  ( 0.000000000000000000, 5.750000000000000000, 0.000000000000000000 ) ) ;
#4372 = AXIS2_PLACEMENT_3D ( 'NONE', #5300, #12406, #4458 ) ;
#4373 = CARTESIAN_POINT ( 'NONE',  ( 3.375021911746136194, 0.9999890441286871656, -0.03364778508493743853 ) ) ;
#4374 = AXIS2_PLACEMENT_3D ( 'NONE', #12841, #8121, #14991 ) ;
#4375 = CYLINDRICAL_SURFACE ( 'NONE', #558, 0.4349999999999999423 ) ;
#4376 = CIRCLE ( 'NONE', #14141, 0.2624999999999997335 ) ;
#4377 = CARTESIAN_POINT ( 'NONE',  ( 3.601417382415921686, 1.056999999999999718, 0.3891265382754439117 ) ) ;
#4378 = DIRECTION ( 'NONE',  ( 0.000000000000000000, 0.000000000000000000, -1.000000000000000000 ) ) ;
#4379 = ORIENTED_EDGE ( 'NONE', *, *, #11949, .F. ) ;
#4380 = AXIS2_PLACEMENT_3D ( 'NONE', #14965, #12579, #953 ) ;
#4381 = EDGE_CURVE ( 'NONE', #1062, #14092, #9001, .T. ) ;
#4382 = FACE_OUTER_BOUND ( 'NONE', #14823, .T. ) ;
#4383 = VECTOR ( 'NONE', #11223, 39.37007874015748143 ) ;
#4384 = ORIENTED_EDGE ( 'NONE', *, *, #3683, .F. ) ;
#4385 = DIRECTION ( 'NONE',  ( 0.000000000000000000, 1.000000000000000000, 0.000000000000000000 ) ) ;
#4386 = CARTESIAN_POINT ( 'NONE',  ( 0.7206835787589728204, -0.4360447880780422003, -0.4581197915133099485 ) ) ;
#4387 = DIRECTION ( 'NONE',  ( 0.000000000000000000, 0.000000000000000000, 1.000000000000000000 ) ) ;
#4388 = VECTOR ( 'NONE', #11030, 39.37007874015748143 ) ;
#4389 = EDGE_CURVE ( 'NONE', #12451, #2938, #6728, .T. ) ;
#4390 = DIRECTION ( 'NONE',  ( 0.000000000000000000, 0.000000000000000000, -1.000000000000000000 ) ) ;
#4391 = VERTEX_POINT ( 'NONE', #11385 ) ;
#4392 = DIRECTION ( 'NONE',  ( 0.7071067811865414665, -0.7071067811865535679, 0.000000000000000000 ) ) ;
#4393 = DIRECTION ( 'NONE',  ( 1.000000000000000000, 0.000000000000000000, 0.000000000000000000 ) ) ;
#4394 = DIRECTION ( 'NONE',  ( 0.000000000000000000, 0.000000000000000000, -1.000000000000000000 ) ) ;
#4395 = EDGE_LOOP ( 'NONE', ( #6595, #11723 ) ) ;
#4396 = ORIENTED_EDGE ( 'NONE', *, *, #1117, .T. ) ;
#4397 = CARTESIAN_POINT ( 'NONE',  ( 2.124999999999999556, 1.679378605318059048, 1.384878605318041744 ) ) ;
#4398 = DIRECTION ( 'NONE',  ( 0.000000000000000000, 0.000000000000000000, 1.000000000000000000 ) ) ;
#4399 = ORIENTED_EDGE ( 'NONE', *, *, #9944, .T. ) ;
#4400 = CARTESIAN_POINT ( 'NONE',  ( 2.774999999999999911, -1.679378605318041950, 1.973878605318057700 ) ) ;
#4401 = EDGE_CURVE ( 'NONE', #2942, #12302, #13369, .T. ) ;
#4402 = CARTESIAN_POINT ( 'NONE',  ( 0.6566194192392912354, -0.4311570606644820614, -0.4974488347804309485 ) ) ;
#4403 = VECTOR ( 'NONE', #13975, 39.37007874015748854 ) ;
#4404 = DIRECTION ( 'NONE',  ( 0.000000000000000000, 0.000000000000000000, -1.000000000000000000 ) ) ;
#4405 = EDGE_CURVE ( 'NONE', #3668, #8487, #2203, .T. ) ;
#4406 = CARTESIAN_POINT ( 'NONE',  ( 2.742999999999999883, -1.679378605318041950, 1.679378605318059048 ) ) ;
#4407 = ORIENTED_EDGE ( 'NONE', *, *, #9714, .F. ) ;
#4408 = DIRECTION ( 'NONE',  ( -1.000000000000000000, -0.000000000000000000, -0.000000000000000000 ) ) ;
#4409 = CARTESIAN_POINT ( 'NONE',  ( 3.843202889607961303, 1.866619761049737702, -0.7500470051816043870 ) ) ;
#4410 = ORIENTED_EDGE ( 'NONE', *, *, #3269, .T. ) ;
#4411 = VERTEX_POINT ( 'NONE', #1041 ) ;
#4412 = CARTESIAN_POINT ( 'NONE',  ( -0.3480941905909599177, 1.602948811930424711, -0.1589886820289102831 ) ) ;
#4413 = ORIENTED_EDGE ( 'NONE', *, *, #697, .F. ) ;
#4414 = CARTESIAN_POINT ( 'NONE',  ( 3.874999999999999556, 3.567999999999999616, 1.509999999999999787 ) ) ;
#4415 = CARTESIAN_POINT ( 'NONE',  ( 2.633946444925666874, 0.3625193201794746356, 0.4033906250602100618 ) ) ;
#4416 = DIRECTION ( 'NONE',  ( 0.000000000000000000, 0.000000000000000000, -1.000000000000000000 ) ) ;
#4417 = CARTESIAN_POINT ( 'NONE',  ( 2.187631780374527324, 0.4716415227047960901, 0.4691012460399078821 ) ) ;
#4418 = ORIENTED_EDGE ( 'NONE', *, *, #8804, .F. ) ;
#4419 = CARTESIAN_POINT ( 'NONE',  ( 6.794491571325179891, -1.679378605318048390, 1.679378605318054163 ) ) ;
#4420 = EDGE_CURVE ( 'NONE', #7408, #9092, #5732, .T. ) ;
#4421 = ADVANCED_FACE ( 'NONE', ( #9257, #12378 ), #11240, .T. ) ;
#4422 = CARTESIAN_POINT ( 'NONE',  ( 0.6570965961311068249, -0.05543357626841138863, -0.5130374278108783548 ) ) ;
#4423 = DIRECTION ( 'NONE',  ( -1.000000000000000000, -0.000000000000000000, -0.000000000000000000 ) ) ;
#4424 = CARTESIAN_POINT ( 'NONE',  ( 4.496007498000189173, 1.789057273259985203, 0.4232163064126445162 ) ) ;
#4426 = VERTEX_POINT ( 'NONE', #8347 ) ;
#4425 = CYLINDRICAL_SURFACE ( 'NONE', #6678, 0.03999999999999998002 ) ;
#4427 = ORIENTED_EDGE ( 'NONE', *, *, #3266, .F. ) ;
#4429 = ORIENTED_EDGE ( 'NONE', *, *, #2248, .T. ) ;
#4428 = CARTESIAN_POINT ( 'NONE',  ( 1.000000000000000000, -0.4429999999999998939, 0.5000000000000000000 ) ) ;
#4430 = ORIENTED_EDGE ( 'NONE', *, *, #4842, .F. ) ;
#4431 = CARTESIAN_POINT ( 'NONE',  ( -0.0008473731076987391477, -0.05999999999999997696, -0.4400059839749300150 ) ) ;
#4432 = DIRECTION ( 'NONE',  ( 1.000000000000000000, 0.000000000000000000, 0.000000000000000000 ) ) ;
#4433 = FACE_OUTER_BOUND ( 'NONE', #9451, .T. ) ;
#4434 = ORIENTED_EDGE ( 'NONE', *, *, #6727, .T. ) ;
#4435 = CARTESIAN_POINT ( 'NONE',  ( 2.774999999999999911, -1.575000000000027489, -1.574999999999989297 ) ) ;
#4436 = CARTESIAN_POINT ( 'NONE',  ( 0.6766651500320096657, -0.4745799178806336949, -0.4479228816209578357 ) ) ;
#4437 = AXIS2_PLACEMENT_3D ( 'NONE', #4886, #400, #11907 ) ;
#4438 = CARTESIAN_POINT ( 'NONE',  ( 3.875000000000619504, 1.884022191776286714, 0.5000000000000002220 ) ) ;
#4439 = DIRECTION ( 'NONE',  ( 0.000000000000000000, 0.000000000000000000, -1.000000000000000000 ) ) ;
#4440 = CARTESIAN_POINT ( 'NONE',  ( 3.083590687937563857, 0.9932358216848905519, -0.4564464592101518114 ) ) ;
#4441 = CARTESIAN_POINT ( 'NONE',  ( -0.2849999999999999756, 4.529999999999999361, -0.4108223460329293864 ) ) ;
#4442 = VERTEX_POINT ( 'NONE', #2443 ) ;
#4443 = DIRECTION ( 'NONE',  ( 0.7071067811865450192, 0.000000000000000000, -0.7071067811865499042 ) ) ;
#4444 = CARTESIAN_POINT ( 'NONE',  ( 3.783833682798621201, 1.905610919832175787, 0.4921549320435091301 ) ) ;
#4445 = CARTESIAN_POINT ( 'NONE',  ( 3.761567849157291921, 1.814885103198726313, -0.7939663826119651713 ) ) ;
#4446 = AXIS2_PLACEMENT_3D ( 'NONE', #5530, #912, #9122 ) ;
#4447 = DIRECTION ( 'NONE',  ( -1.000000000000000000, -0.000000000000000000, -0.000000000000000000 ) ) ;
#4449 = ORIENTED_EDGE ( 'NONE', *, *, #6068, .T. ) ;
#4448 = DIRECTION ( 'NONE',  ( 1.000000000000000000, 0.000000000000000000, -1.655665450705613915E-16 ) ) ;
#4450 = VERTEX_POINT ( 'NONE', #8186 ) ;
#4451 = DIRECTION ( 'NONE',  ( -1.000000000000000000, -0.000000000000000000, -0.000000000000000000 ) ) ;
#4452 = VERTEX_POINT ( 'NONE', #12749 ) ;
#4453 = ADVANCED_FACE ( 'NONE', ( #6034, #3588, #5957, #1345 ), #2275, .F. ) ;
#4454 = FACE_OUTER_BOUND ( 'NONE', #9650, .T. ) ;
#4455 = DIRECTION ( 'NONE',  ( -1.000000000000000000, -0.000000000000000000, -0.000000000000000000 ) ) ;
#4456 = LINE ( 'NONE', #10196, #12253 ) ;
#4457 = CARTESIAN_POINT ( 'NONE',  ( 3.874999999999999556, 2.782000000000000917, -1.320000000000000062 ) ) ;
#4458 = DIRECTION ( 'NONE',  ( 0.000000000000000000, 0.000000000000000000, -1.000000000000000000 ) ) ;
#4459 = ORIENTED_EDGE ( 'NONE', *, *, #3818, .F. ) ;
#4460 = CARTESIAN_POINT ( 'NONE',  ( -0.3725000000000002198, 0.1859999999999983611, -0.3725000000000000533 ) ) ;
#4461 = CARTESIAN_POINT ( 'NONE',  ( 0.8254245316410396827, -0.4829999999999998739, -0.3670313414528085239 ) ) ;
#4462 = CARTESIAN_POINT ( 'NONE',  ( 2.742999999999999883, -1.679378605318041950, 1.679378605318059048 ) ) ;
#4463 = ORIENTED_EDGE ( 'NONE', *, *, #10825, .F. ) ;
#4464 = VECTOR ( 'NONE', #14612, 39.37007874015748143 ) ;
#4465 = DIRECTION ( 'NONE',  ( 0.000000000000000000, 1.224646799147354933E-16, 1.000000000000000000 ) ) ;
#4466 = EDGE_LOOP ( 'NONE', ( #8818, #11285 ) ) ;
#4467 = CARTESIAN_POINT ( 'NONE',  ( 0.000000000000000000, 1.239999999999999991, 0.000000000000000000 ) ) ;
#4468 = EDGE_CURVE ( 'NONE', #15151, #5693, #12827, .T. ) ;
#4469 = CARTESIAN_POINT ( 'NONE',  ( 0.6732025385091796599, -0.3978263200806930744, -0.4888865340280575400 ) ) ;
#4470 = ADVANCED_FACE ( 'NONE', ( #5809 ), #1271, .T. ) ;
#4471 = CARTESIAN_POINT ( 'NONE',  ( 0.8999999999999999112, -0.6429999999999999050, -0.3750000000000000555 ) ) ;
#4472 = CARTESIAN_POINT ( 'NONE',  ( 3.715407914194799766, 1.936056580808199312, 0.4744061610882758240 ) ) ;
#4473 = AXIS2_PLACEMENT_3D ( 'NONE', #10459, #13731, #4495 ) ;
#4474 = EDGE_CURVE ( 'NONE', #5449, #4107, #7020, .T. ) ;
#4475 = ORIENTED_EDGE ( 'NONE', *, *, #8058, .T. ) ;
#4476 = EDGE_CURVE ( 'NONE', #13120, #10897, #11698, .T. ) ;
#4477 = CIRCLE ( 'NONE', #6199, 1.039370078740158965 ) ;
#4478 = ORIENTED_EDGE ( 'NONE', *, *, #5401, .T. ) ;
#4479 = ORIENTED_EDGE ( 'NONE', *, *, #14933, .T. ) ;
#4480 = UNCERTAINTY_MEASURE_WITH_UNIT (LENGTH_MEASURE( 1.000000000000000082E-05 ), #321, 'distance_accuracy_value', 'NONE');
#4481 = CARTESIAN_POINT ( 'NONE',  ( -0.2577064312470127572, 1.589827634136290468, -0.3155448735949362149 ) ) ;
#4482 = ORIENTED_EDGE ( 'NONE', *, *, #2418, .T. ) ;
#4483 = DIRECTION ( 'NONE',  ( 0.000000000000000000, 1.000000000000000000, 0.000000000000000000 ) ) ;
#4484 = DIRECTION ( 'NONE',  ( -1.000000000000000000, -0.000000000000000000, -0.000000000000000000 ) ) ;
#4485 = DIRECTION ( 'NONE',  ( 0.000000000000000000, 0.000000000000000000, -1.000000000000000000 ) ) ;
#4486 = CARTESIAN_POINT ( 'NONE',  ( 0.1266950372298308314, 1.593635284016129416, -0.3809527529760087239 ) ) ;
#4487 = VERTEX_POINT ( 'NONE', #1199 ) ;
#4488 = DIRECTION ( 'NONE',  ( 0.000000000000000000, 0.7071067811865603403, 0.7071067811865345831 ) ) ;
#4489 = CARTESIAN_POINT ( 'NONE',  ( 0.6558154374103656314, -0.01854616410104658816, -0.5012742423172328321 ) ) ;
#4490 = CONICAL_SURFACE ( 'NONE', #791, 0.2624999999999852451, 0.7853981633974428389 ) ;
#4491 =( CONVERSION_BASED_UNIT ( 'INCH', #9086 ) LENGTH_UNIT ( ) NAMED_UNIT ( #11056 ) );
#4492 = EDGE_CURVE ( 'NONE', #6235, #7135, #5797, .T. ) ;
#4493 = CIRCLE ( 'NONE', #9863, 0.06999999999999836908 ) ;
#4494 = ADVANCED_FACE ( 'NONE', ( #14132 ), #10697, .F. ) ;
#4495 = DIRECTION ( 'NONE',  ( -1.000000000000000000, -1.365923996832131609E-16, 0.000000000000000000 ) ) ;
#4496 = CARTESIAN_POINT ( 'NONE',  ( 4.613894443967907044, 1.807937564491455262, -0.1419188128446503272 ) ) ;
#4498 = ORIENTED_EDGE ( 'NONE', *, *, #1639, .T. ) ;
#4497 = FACE_BOUND ( 'NONE', #6368, .T. ) ;
#4499 = ADVANCED_FACE ( 'NONE', ( #10621 ), #8269, .T. ) ;
#4500 = APPLICATION_CONTEXT ( 'automotive_design' ) ;
#4501 = ORIENTED_EDGE ( 'NONE', *, *, #6372, .T. ) ;
#4503 = ORIENTED_EDGE ( 'NONE', *, *, #1311, .T. ) ;
#4502 = CARTESIAN_POINT ( 'NONE',  ( 3.061616997868382402E-17, 0.000000000000000000, 0.2499999999999999167 ) ) ;
#4504 = ORIENTED_EDGE ( 'NONE', *, *, #14877, .F. ) ;
#4505 = AXIS2_PLACEMENT_3D ( 'NONE', #11699, #8109, #2276 ) ;
#4506 = DIRECTION ( 'NONE',  ( 0.000000000000000000, 0.000000000000000000, 1.000000000000000000 ) ) ;
#4507 = DIRECTION ( 'NONE',  ( 0.000000000000000000, 0.000000000000000000, 1.000000000000000000 ) ) ;
#4508 = DIRECTION ( 'NONE',  ( 0.000000000000000000, 0.000000000000000000, -1.000000000000000000 ) ) ;
#4509 = VERTEX_POINT ( 'NONE', #9561 ) ;
#4510 = DIRECTION ( 'NONE',  ( 0.7071067811865523467, 8.659560562354873694E-17, 0.7071067811865425767 ) ) ;
#4511 = CARTESIAN_POINT ( 'NONE',  ( 2.001999999999999780, 0.000000000000000000, 1.350000000000000089 ) ) ;
#4512 = DIRECTION ( 'NONE',  ( -0.000000000000000000, -1.000000000000000000, -0.000000000000000000 ) ) ;
#4513 = AXIS2_PLACEMENT_3D ( 'NONE', #6207, #508, #2907 ) ;
#4514 = CARTESIAN_POINT ( 'NONE',  ( 0.7058998964907862161, -0.3830000000000000071, -0.4900296624789436950 ) ) ;
#4515 = DIRECTION ( 'NONE',  ( -0.000000000000000000, -1.000000000000000000, 0.000000000000000000 ) ) ;
#4516 = CARTESIAN_POINT ( 'NONE',  ( 0.09500000000000168032, 0.000000000000000000, 0.000000000000000000 ) ) ;
#4517 = CARTESIAN_POINT ( 'NONE',  ( 3.652526911380074903, 0.8940386994653520825, 0.4480710255186519109 ) ) ;
#4518 = CARTESIAN_POINT ( 'NONE',  ( 0.09500000000000431710, -1.679378605318048390, 1.679378605318054163 ) ) ;
#4519 = EDGE_CURVE ( 'NONE', #5884, #14900, #385, .T. ) ;
#4520 = FACE_OUTER_BOUND ( 'NONE', #5132, .T. ) ;
#4522 = ORIENTED_EDGE ( 'NONE', *, *, #12317, .F. ) ;
#4521 = FACE_BOUND ( 'NONE', #13820, .T. ) ;
#4523 = EDGE_LOOP ( 'NONE', ( #1637, #7905, #3174, #9326 ) ) ;
#4524 = AXIS2_PLACEMENT_3D ( 'NONE', #1736, #12081, #9865 ) ;
#4525 = LINE ( 'NONE', #9197, #1550 ) ;
#4526 = ORIENTED_EDGE ( 'NONE', *, *, #13034, .T. ) ;
#4527 = FACE_OUTER_BOUND ( 'NONE', #11271, .T. ) ;
#4528 = AXIS2_PLACEMENT_3D ( 'NONE', #165, #4867, #9605 ) ;
#4529 = VECTOR ( 'NONE', #2232, 39.37007874015748143 ) ;
#4530 = CARTESIAN_POINT ( 'NONE',  ( 3.250637184708968785, 0.6799532182389171897, -0.4540870454137406198 ) ) ;
#4531 = CARTESIAN_POINT ( 'NONE',  ( 2.220468100499050745, -0.03283382702752232762, 0.4686374562078457484 ) ) ;
#4532 = DIRECTION ( 'NONE',  ( -0.000000000000000000, -1.000000000000000000, -0.000000000000000000 ) ) ;
#4533 = DIRECTION ( 'NONE',  ( -1.000000000000000000, 0.000000000000000000, 0.000000000000000000 ) ) ;
#4534 = EDGE_LOOP ( 'NONE', ( #3410, #2278, #12350, #9540 ) ) ;
#4535 = CIRCLE ( 'NONE', #10402, 0.3750000000000004996 ) ;
#4536 = CARTESIAN_POINT ( 'NONE',  ( 0.6555160077358691550, -0.4028346421833865487, 0.5098802871450707208 ) ) ;
#4537 = FACE_OUTER_BOUND ( 'NONE', #1467, .T. ) ;
#4538 = CIRCLE ( 'NONE', #13077, 0.9999999999999998890 ) ;
#4539 = AXIS2_PLACEMENT_3D ( 'NONE', #6745, #14766, #904 ) ;
#4540 = EDGE_LOOP ( 'NONE', ( #4658, #4645, #13026, #12282 ) ) ;
#4541 = LINE ( 'NONE', #2239, #3249 ) ;
#4542 = ADVANCED_FACE ( 'NONE', ( #10546 ), #149, .F. ) ;
#4543 = ORIENTED_EDGE ( 'NONE', *, *, #3949, .F. ) ;
#4544 = CARTESIAN_POINT ( 'NONE',  ( 3.426491571325181340, -1.679378605318041950, 1.973878605318057700 ) ) ;
#4545 = LINE ( 'NONE', #9372, #10596 ) ;
#4546 = EDGE_LOOP ( 'NONE', ( #14768, #13484 ) ) ;
#4547 = CARTESIAN_POINT ( 'NONE',  ( 3.113342878570761307, 0.6489923502455474669, 0.4560262305287002826 ) ) ;
#4548 = PLANE ( 'NONE',  #9181 ) ;
#4549 = VECTOR ( 'NONE', #9113, 39.37007874015748854 ) ;
#4550 = DIRECTION ( 'NONE',  ( 0.000000000000000000, 1.000000000000000000, 0.000000000000000000 ) ) ;
#4551 = AXIS2_PLACEMENT_3D ( 'NONE', #10283, #9135, #4465 ) ;
#4552 = CARTESIAN_POINT ( 'NONE',  ( 6.794491571325179891, 1.679378605318035733, -2.054378605318066153 ) ) ;
#4553 = LINE ( 'NONE', #9224, #14548 ) ;
#4554 = ADVANCED_FACE ( 'NONE', ( #7188 ), #3504, .T. ) ;
#4555 = EDGE_CURVE ( 'NONE', #5428, #12577, #7366, .T. ) ;
#4556 = CIRCLE ( 'NONE', #13096, 0.9499999999999992895 ) ;
#4557 = ADVANCED_FACE ( 'NONE', ( #633 ), #14086, .F. ) ;
#4558 = CARTESIAN_POINT ( 'NONE',  ( 3.933597127675186211, 1.764057874260432701, -0.7948317876848067787 ) ) ;
#4559 = VERTEX_POINT ( 'NONE', #6478 ) ;
#4560 = ORIENTED_EDGE ( 'NONE', *, *, #6861, .T. ) ;
#4561 = DIRECTION ( 'NONE',  ( -0.9992912762382413216, -0.03489602031262311471, 0.01411428356268702201 ) ) ;
#4562 = EDGE_LOOP ( 'NONE', ( #13092, #6013 ) ) ;
#4563 = DIRECTION ( 'NONE',  ( 0.000000000000000000, 1.000000000000000000, -0.000000000000000000 ) ) ;
#4564 = LINE ( 'NONE', #1327, #7860 ) ;
#4565 = CARTESIAN_POINT ( 'NONE',  ( -0.09035531712817639061, 1.379999999999999671, -0.1564999999999998892 ) ) ;
#4566 = ADVANCED_FACE ( 'NONE', ( #14492 ), #11135, .F. ) ;
#4567 = DIRECTION ( 'NONE',  ( 1.365923996832131609E-16, -1.000000000000000000, 0.000000000000000000 ) ) ;
#4568 = ORIENTED_EDGE ( 'NONE', *, *, #2413, .T. ) ;
#4569 = CARTESIAN_POINT ( 'NONE',  ( 3.154159632798697377, 2.491856171652469421, 0.2021108258708759486 ) ) ;
#4570 = AXIS2_PLACEMENT_3D ( 'NONE', #15035, #6016, #2337 ) ;
#4571 = CARTESIAN_POINT ( 'NONE',  ( 0.7070627455984020981, -0.01874658262850352822, -0.4737642524341751926 ) ) ;
#4572 = CARTESIAN_POINT ( 'NONE',  ( 1.250847373107698779, -0.05999999999999997696, -0.4823326642216426707 ) ) ;
#4573 = CIRCLE ( 'NONE', #13334, 1.000000000000000222 ) ;
#4574 = DIRECTION ( 'NONE',  ( -1.000000000000000000, -0.000000000000000000, -0.000000000000000000 ) ) ;
#4575 = CARTESIAN_POINT ( 'NONE',  ( 4.564206621729743674, 1.716523463454355358, -0.4148897219068747311 ) ) ;
#4577 = VERTEX_POINT ( 'NONE', #7475 ) ;
#4576 = DIRECTION ( 'NONE',  ( -0.000000000000000000, -1.000000000000000000, -0.000000000000000000 ) ) ;
#4578 = AXIS2_PLACEMENT_3D ( 'NONE', #12045, #5093, #12197 ) ;
#4579 = ORIENTED_EDGE ( 'NONE', *, *, #14681, .F. ) ;
#4581 = ORIENTED_EDGE ( 'NONE', *, *, #12163, .F. ) ;
#4580 = FACE_OUTER_BOUND ( 'NONE', #10386, .T. ) ;
#4582 = ORIENTED_EDGE ( 'NONE', *, *, #1324, .T. ) ;
#4583 = FACE_OUTER_BOUND ( 'NONE', #12959, .T. ) ;
#4584 = DIRECTION ( 'NONE',  ( 1.000000000000000000, 0.000000000000000000, 0.000000000000000000 ) ) ;
#4585 = DIRECTION ( 'NONE',  ( 1.000000000000000000, 0.000000000000000000, 0.000000000000000000 ) ) ;
#4586 = ORIENTED_EDGE ( 'NONE', *, *, #12770, .T. ) ;
#4587 = DIRECTION ( 'NONE',  ( 0.9999002670844989726, -2.665865973017557838E-15, -0.01412288512831216640 ) ) ;
#4588 = CARTESIAN_POINT ( 'NONE',  ( 2.774999999999999911, -3.360000000000000320, 0.9799999999999999822 ) ) ;
#4589 = AXIS2_PLACEMENT_3D ( 'NONE', #8952, #6890, #4587 ) ;
#4590 = EDGE_CURVE ( 'NONE', #1534, #9323, #12860, .T. ) ;
#4591 = PLANE ( 'NONE',  #9041 ) ;
#4592 = EDGE_CURVE ( 'NONE', #5059, #3954, #1642, .T. ) ;
#4593 = CARTESIAN_POINT ( 'NONE',  ( 3.601417382415921686, 1.056999999999999718, 0.3891265382754439117 ) ) ;
#4594 = CONICAL_SURFACE ( 'NONE', #5821, 0.07000000000000047851, 0.7853981633974297383 ) ;
#4595 = DIRECTION ( 'NONE',  ( 0.000000000000000000, 0.000000000000000000, 1.000000000000000000 ) ) ;
#4596 = CARTESIAN_POINT ( 'NONE',  ( 3.874999999999999556, 3.137999999999999901, 1.542000000000000037 ) ) ;
#4597 = CARTESIAN_POINT ( 'NONE',  ( 8.792093969802149189, 0.8799778768672790186, 6.829619984160658046E-17 ) ) ;
#4598 = CIRCLE ( 'NONE', #12640, 0.9499999999999988454 ) ;
#4599 = PLANE ( 'NONE',  #4005 ) ;
#4600 = DIRECTION ( 'NONE',  ( 0.000000000000000000, 0.000000000000000000, 1.000000000000000000 ) ) ;
#4602 = ORIENTED_EDGE ( 'NONE', *, *, #8488, .F. ) ;
#4601 = PLANE ( 'NONE',  #5529 ) ;
#4603 = ORIENTED_EDGE ( 'NONE', *, *, #9379, .T. ) ;
#4604 = CARTESIAN_POINT ( 'NONE',  ( 0.6592591305498912702, 0.0007908075296091682943, -0.4883895785410080626 ) ) ;
#4605 = VERTEX_POINT ( 'NONE', #1568 ) ;
#4606 = AXIS2_PLACEMENT_3D ( 'NONE', #10763, #317, #2793 ) ;
#4607 = CARTESIAN_POINT ( 'NONE',  ( 3.875000000000000000, 3.137999999999999901, 0.000000000000000000 ) ) ;
#4608 = AXIS2_PLACEMENT_3D ( 'NONE', #8649, #6587, #11245 ) ;
#4609 = CARTESIAN_POINT ( 'NONE',  ( 2.916325821605861623, 0.5706613545855859781, -0.3991895006237661803 ) ) ;
#4610 = EDGE_CURVE ( 'NONE', #12651, #8027, #14348, .T. ) ;
#4611 = EDGE_CURVE ( 'NONE', #2093, #8372, #14816, .T. ) ;
#4612 = DIRECTION ( 'NONE',  ( 0.000000000000000000, 1.000000000000000000, 0.000000000000000000 ) ) ;
#4613 = VECTOR ( 'NONE', #13176, 39.37007874015748143 ) ;
#4614 = CIRCLE ( 'NONE', #13375, 0.7173254825712085392 ) ;
#4615 = DIRECTION ( 'NONE',  ( -1.000000000000000000, -0.000000000000000000, -0.000000000000000000 ) ) ;
#4616 = CIRCLE ( 'NONE', #917, 1.502725933896874810 ) ;
#4617 = EDGE_LOOP ( 'NONE', ( #14075, #1003, #3044, #10467, #3253, #11896, #5625, #5414, #3926, #9448, #12228 ) ) ;
#4618 = AXIS2_PLACEMENT_3D ( 'NONE', #10579, #7155, #11880 ) ;
#4619 = CARTESIAN_POINT ( 'NONE',  ( 0.7073375012244004223, -0.4456044010854968151, 0.4168187156545198335 ) ) ;
#4620 = DIRECTION ( 'NONE',  ( 0.000000000000000000, 0.000000000000000000, -1.000000000000000000 ) ) ;
#4621 = ORIENTED_EDGE ( 'NONE', *, *, #3817, .F. ) ;
#4622 = VECTOR ( 'NONE', #8416, 39.37007874015748143 ) ;
#4623 = CARTESIAN_POINT ( 'NONE',  ( 0.7513246802501661881, -0.4429999999999998939, -0.4293820849162031661 ) ) ;
#4624 = ORIENTED_EDGE ( 'NONE', *, *, #831, .F. ) ;
#4625 = CARTESIAN_POINT ( 'NONE',  ( 0.6500000000000001332, -1.679378605318048390, 2.086378605318058632 ) ) ;
#4626 = VERTEX_POINT ( 'NONE', #8483 ) ;
#4627 = AXIS2_PLACEMENT_3D ( 'NONE', #2618, #291, #8371 ) ;
#4628 = LINE ( 'NONE', #11811, #7237 ) ;
#4629 = AXIS2_PLACEMENT_3D ( 'NONE', #5642, #11523, #4485 ) ;
#4630 = DIRECTION ( 'NONE',  ( 1.000000000000000000, -2.602462600580852055E-17, 0.000000000000000000 ) ) ;
#4631 = AXIS2_PLACEMENT_3D ( 'NONE', #13033, #4799, #252 ) ;
#4632 = CARTESIAN_POINT ( 'NONE',  ( 4.203919238849069373, 1.786011173657954476, -0.6749003061560150396 ) ) ;
#4633 = EDGE_CURVE ( 'NONE', #7622, #7601, #5299, .T. ) ;
#4634 = DIRECTION ( 'NONE',  ( 0.8660254037844362651, 0.000000000000000000, -0.5000000000000041078 ) ) ;
#4635 = AXIS2_PLACEMENT_3D ( 'NONE', #8212, #5837, #12542 ) ;
#4636 = VERTEX_POINT ( 'NONE', #7548 ) ;
#4637 = ORIENTED_EDGE ( 'NONE', *, *, #1577, .F. ) ;
#4638 = VECTOR ( 'NONE', #14016, 39.37007874015748143 ) ;
#4639 = CARTESIAN_POINT ( 'NONE',  ( 0.000000000000000000, 5.750000000000000000, 0.000000000000000000 ) ) ;
#4640 = ORIENTED_EDGE ( 'NONE', *, *, #12110, .F. ) ;
#4641 = CARTESIAN_POINT ( 'NONE',  ( 0.4349147617188408588, 1.559103846021540951, -0.008611041693278118775 ) ) ;
#4642 = CARTESIAN_POINT ( 'NONE',  ( 4.315797241329101475, 3.137999999999999901, 1.570821732971949825 ) ) ;
#4643 = CARTESIAN_POINT ( 'NONE',  ( 6.123233995736762338E-17, 1.866025403784438819, 0.4999999999999995004 ) ) ;
#4644 = DIRECTION ( 'NONE',  ( 0.000000000000000000, 0.000000000000000000, -1.000000000000000000 ) ) ;
#4645 = ORIENTED_EDGE ( 'NONE', *, *, #6743, .F. ) ;
#4646 = CARTESIAN_POINT ( 'NONE',  ( 3.150340687203102341, 2.492967108137689181, 0.1879335863375432569 ) ) ;
#4647 = EDGE_CURVE ( 'NONE', #6033, #12028, #5330, .T. ) ;
#4648 = CARTESIAN_POINT ( 'NONE',  ( 0.6742552310713034736, -0.02516590133966824933, -0.4797493044159580888 ) ) ;
#4649 = EDGE_CURVE ( 'NONE', #6882, #8178, #873, .T. ) ;
#4650 = FACE_OUTER_BOUND ( 'NONE', #8558, .T. ) ;
#4651 = EDGE_CURVE ( 'NONE', #14886, #13231, #11403, .T. ) ;
#4652 = CARTESIAN_POINT ( 'NONE',  ( 4.574338115621504386, 1.717610331383472744, -0.3985571411410331333 ) ) ;
#4653 = ORIENTED_EDGE ( 'NONE', *, *, #2180, .F. ) ;
#4655 = ORIENTED_EDGE ( 'NONE', *, *, #9452, .T. ) ;
#4654 = CARTESIAN_POINT ( 'NONE',  ( 0.2665675396067855862, 1.593633255602470156, 0.3001969837044382028 ) ) ;
#4656 = ORIENTED_EDGE ( 'NONE', *, *, #383, .F. ) ;
#4658 = ORIENTED_EDGE ( 'NONE', *, *, #10181, .T. ) ;
#4657 = LINE ( 'NONE', #3737, #10186 ) ;
#4659 = ORIENTED_EDGE ( 'NONE', *, *, #4030, .T. ) ;
#4660 = DIRECTION ( 'NONE',  ( 0.000000000000000000, 0.000000000000000000, -1.000000000000000000 ) ) ;
#4661 = DIRECTION ( 'NONE',  ( 0.000000000000000000, 0.000000000000000000, 1.000000000000000000 ) ) ;
#4662 = FACE_OUTER_BOUND ( 'NONE', #9856, .T. ) ;
#4663 =( BOUNDED_SURFACE ( )  B_SPLINE_SURFACE ( 3, 2, ( 
 ( #393, #5233, #12263 ),
 ( #8609, #9757, #538 ),
 ( #11116, #11042, #4087 ),
 ( #1482, #4011, #13404 ),
 ( #8676, #2941, #619 ),
 ( #6389, #2790, #7390 ),
 ( #2861, #9685, #9902 ),
 ( #13322, #7602, #7528 ),
 ( #9985, #6165, #14333 ),
 ( #3790, #10824, #8466 ) ),
 .UNSPECIFIED., .F., .F., .F. ) 
 B_SPLINE_SURFACE_WITH_KNOTS ( ( 4, 2, 2, 2, 4 ),
 ( 3, 3 ),
 ( 0.000000000000000000, 0.3891682430355878353, 0.7783364860711756705, 1.167504729106763506, 1.556672972142351341 ),
 ( 0.000000000000000000, 1.000000000000000000 ),
 .UNSPECIFIED. ) 
 GEOMETRIC_REPRESENTATION_ITEM ( )  RATIONAL_B_SPLINE_SURFACE ( (
 ( 1.000000000000000000, 0.7193398003386451967, 1.000000000000000000),
 ( 1.000000000000000000, 0.7193411551263428905, 1.000000000000000000),
 ( 1.000000000000000000, 0.7190300160696043719, 1.000000000000000000),
 ( 1.000000000000000000, 0.7178345465032389683, 1.000000000000000000),
 ( 1.000000000000000000, 0.7169492149876324216, 1.000000000000000000),
 ( 1.000000000000000000, 0.7147290448015459763, 1.000000000000000000),
 ( 1.000000000000000000, 0.7133949008891797838, 1.000000000000000000),
 ( 1.000000000000000000, 0.7104704279355633645, 1.000000000000000000),
 ( 1.000000000000000000, 0.7088814831338368094, 1.000000000000000000),
 ( 1.000000000000000000, 0.7072810196742753686, 1.000000000000000000) ) ) 
 REPRESENTATION_ITEM ( '' )  SURFACE ( )  );
#4664 = ORIENTED_EDGE ( 'NONE', *, *, #7466, .T. ) ;
#4665 = DIRECTION ( 'NONE',  ( 1.000000000000000000, -2.602462600580852055E-17, 0.000000000000000000 ) ) ;
#4666 = CYLINDRICAL_SURFACE ( 'NONE', #8526, 1.000000000000000000 ) ;
#4667 = EDGE_CURVE ( 'NONE', #14527, #4100, #8622, .T. ) ;
#4668 = CARTESIAN_POINT ( 'NONE',  ( 3.874999999999999556, 3.137999999999999901, 1.097500000000000586 ) ) ;
#4669 = ADVANCED_FACE ( 'NONE', ( #8560 ), #13833, .T. ) ;
#4670 = DIRECTION ( 'NONE',  ( 0.000000000000000000, 0.000000000000000000, -1.000000000000000000 ) ) ;
#4671=STYLED_ITEM('',(#15171),#5584);
#4672 = DIRECTION ( 'NONE',  ( -1.000000000000000000, -1.874307916738609066E-16, 0.000000000000000000 ) ) ;
#4673 = FACE_OUTER_BOUND ( 'NONE', #6906, .T. ) ;
#4674 = CARTESIAN_POINT ( 'NONE',  ( 2.774999999999999911, 1.679378605318059048, 1.941878605318041240 ) ) ;
#4675 = DIRECTION ( 'NONE',  ( 1.000000000000000000, 0.000000000000000000, 0.000000000000000000 ) ) ;
#4676 = CARTESIAN_POINT ( 'NONE',  ( 4.449790221757562669, 1.708297502301393544, 0.5563949201538650469 ) ) ;
#4677 = ADVANCED_FACE ( 'NONE', ( #5113 ), #7405, .T. ) ;
#4678 = ORIENTED_EDGE ( 'NONE', *, *, #6485, .F. ) ;
#4679 = DIRECTION ( 'NONE',  ( 0.000000000000000000, 0.000000000000000000, -1.000000000000000000 ) ) ;
#4681 = ORIENTED_EDGE ( 'NONE', *, *, #11288, .F. ) ;
#4680 = LINE ( 'NONE', #4754, #603 ) ;
#4682 = ORIENTED_EDGE ( 'NONE', *, *, #13600, .F. ) ;
#4683 = CARTESIAN_POINT ( 'NONE',  ( 0.7067472695984847730, -0.3830000000000000071, -0.5500236785040135690 ) ) ;
#4684 = EDGE_CURVE ( 'NONE', #5884, #13214, #4104, .T. ) ;
#4685 = LINE ( 'NONE', #9431, #2027 ) ;
#4686 = EDGE_LOOP ( 'NONE', ( #12172, #10059, #13354, #1370 ) ) ;
#4687 = CIRCLE ( 'NONE', #740, 1.000000000000000000 ) ;
#4688 = DIRECTION ( 'NONE',  ( 0.000000000000000000, 0.000000000000000000, -1.000000000000000000 ) ) ;
#4689 = LINE ( 'NONE', #8217, #7940 ) ;
#4690 = DIRECTION ( 'NONE',  ( 0.000000000000000000, 0.000000000000000000, 1.000000000000000000 ) ) ;
#4691 = ADVANCED_FACE ( 'NONE', ( #8776 ), #5249, .T. ) ;
#4692 = ORIENTED_EDGE ( 'NONE', *, *, #9251, .T. ) ;
#4693 = CARTESIAN_POINT ( 'NONE',  ( 0.6746175797782828498, -0.3871287346720767020, 0.4907030699472766377 ) ) ;
#4694 = CIRCLE ( 'NONE', #2246, 0.6700292969071726112 ) ;
#4695 = DIRECTION ( 'NONE',  ( 0.000000000000000000, 0.000000000000000000, -1.000000000000000000 ) ) ;
#4696 = DIRECTION ( 'NONE',  ( -1.000000000000000000, 0.000000000000000000, 0.000000000000000000 ) ) ;
#4697 = VERTEX_POINT ( 'NONE', #12279 ) ;
#4698 = CARTESIAN_POINT ( 'NONE',  ( 6.176491571325181340, 0.000000000000000000, 0.000000000000000000 ) ) ;
#4699 = ORIENTED_EDGE ( 'NONE', *, *, #13488, .F. ) ;
#4700 = EDGE_CURVE ( 'NONE', #8801, #8372, #10191, .T. ) ;
#4701 = FACE_OUTER_BOUND ( 'NONE', #3430, .T. ) ;
#4702 = ORIENTED_EDGE ( 'NONE', *, *, #5294, .F. ) ;
#4703 = DIRECTION ( 'NONE',  ( 0.000000000000000000, 1.000000000000000000, -1.224646799147353207E-16 ) ) ;
#4704 = CARTESIAN_POINT ( 'NONE',  ( 2.002892399651176714, -0.1783233198227758276, -0.4717105593270736752 ) ) ;
#4705 = DIRECTION ( 'NONE',  ( 1.000000000000000000, 0.000000000000000000, 0.000000000000000000 ) ) ;
#4706 = APPLICATION_CONTEXT ( 'automotive_design' ) ;
#4707 = DIRECTION ( 'NONE',  ( 0.000000000000000000, 1.000000000000000000, -0.000000000000000000 ) ) ;
#4708 = AXIS2_PLACEMENT_3D ( 'NONE', #75, #8376, #1305 ) ;
#4709 = ORIENTED_EDGE ( 'NONE', *, *, #7315, .F. ) ;
#4710 = ORIENTED_EDGE ( 'NONE', *, *, #12531, .F. ) ;
#4711 = ADVANCED_FACE ( 'NONE', ( #7925 ), #3333, .T. ) ;
#4712 = LINE ( 'NONE', #3719, #14796 ) ;
#4713 = ORIENTED_EDGE ( 'NONE', *, *, #4316, .T. ) ;
#4714 = DIRECTION ( 'NONE',  ( -1.000000000000000000, -0.000000000000000000, -0.000000000000000000 ) ) ;
#4715 = PRODUCT_DEFINITION ( 'UNKNOWN', '', #13046, #14884 ) ;
#4716 = VECTOR ( 'NONE', #10931, 39.37007874015748143 ) ;
#4717 = CARTESIAN_POINT ( 'NONE',  ( 2.372634528609593563, 0.1852128444980908617, 0.4664882128727458888 ) ) ;
#4718 = CARTESIAN_POINT ( 'NONE',  ( 0.7038870757886633855, -0.05564421503643584427, -0.4900580921498777776 ) ) ;
#4719 = VERTEX_POINT ( 'NONE', #10151 ) ;
#4720 = FACE_OUTER_BOUND ( 'NONE', #13211, .T. ) ;
#4721 = VECTOR ( 'NONE', #4079, 39.37007874015748854 ) ;
#4722 = CARTESIAN_POINT ( 'NONE',  ( 1.249999999999999778, 9.390727478220904197E-17, 0.4223386481965726857 ) ) ;
#4723 = CARTESIAN_POINT ( 'NONE',  ( 2.774999999999999911, 2.360000000000015863, 0.9799999999999454703 ) ) ;
#4724 = CIRCLE ( 'NONE', #9848, 1.350000000000000089 ) ;
#4725 = DIRECTION ( 'NONE',  ( 0.000000000000000000, 0.000000000000000000, 1.000000000000000000 ) ) ;
#4726 = CARTESIAN_POINT ( 'NONE',  ( 4.551166761458199872, 1.796655256677337942, -0.3282260880885092269 ) ) ;
#4727 = VERTEX_POINT ( 'NONE', #5641 ) ;
#4729 = ORIENTED_EDGE ( 'NONE', *, *, #2872, .T. ) ;
#4728 = CARTESIAN_POINT ( 'NONE',  ( 0.3930894239865358464, 1.593697031032150102, 0.08105465168935101217 ) ) ;
#4730 = EDGE_LOOP ( 'NONE', ( #14344, #2939, #27, #4102 ) ) ;
#4731 = DIRECTION ( 'NONE',  ( 0.000000000000000000, 0.000000000000000000, -1.000000000000000000 ) ) ;
#4732 = ORIENTED_EDGE ( 'NONE', *, *, #422, .T. ) ;
#4733 = CARTESIAN_POINT ( 'NONE',  ( 0.000000000000000000, 1.239999999999999991, 0.000000000000000000 ) ) ;
#4734 = CARTESIAN_POINT ( 'NONE',  ( 3.876734730694346265, 3.530000000000000693, -0.001618565749189758169 ) ) ;
#4735 = FACE_OUTER_BOUND ( 'NONE', #10209, .T. ) ;
#4736 = ORIENTED_EDGE ( 'NONE', *, *, #7036, .T. ) ;
#4737 = VECTOR ( 'NONE', #8116, 39.37007874015748143 ) ;
#4738 = DIRECTION ( 'NONE',  ( 0.000000000000000000, 0.000000000000000000, 1.000000000000000000 ) ) ;
#4739 = FACE_OUTER_BOUND ( 'NONE', #13425, .T. ) ;
#4740 = CIRCLE ( 'NONE', #1047, 0.2944999999999998175 ) ;
#4741 = DIRECTION ( 'NONE',  ( 0.000000000000000000, 1.000000000000000000, 0.000000000000000000 ) ) ;
#4742 = CARTESIAN_POINT ( 'NONE',  ( 3.426491571325181340, 0.7000000000000026201, 2.400000000000000355 ) ) ;
#4743 = CARTESIAN_POINT ( 'NONE',  ( 3.405153689607044232, 3.567999999999999616, -1.491010071662831171 ) ) ;
#4744 = LINE ( 'NONE', #12607, #10718 ) ;
#4745 = AXIS2_PLACEMENT_3D ( 'NONE', #1816, #2914, #12306 ) ;
#4746 = FACE_OUTER_BOUND ( 'NONE', #9753, .T. ) ;
#4747 = EDGE_CURVE ( 'NONE', #1386, #14655, #14808, .T. ) ;
#4748 = CARTESIAN_POINT ( 'NONE',  ( 2.229630226914017133, 0.4287871555018993308, 0.4085020630706684974 ) ) ;
#4749 = AXIS2_PLACEMENT_3D ( 'NONE', #10472, #9333, #4432 ) ;
#4750 = EDGE_CURVE ( 'NONE', #9866, #651, #4573, .T. ) ;
#4751 = EDGE_LOOP ( 'NONE', ( #5895, #907, #9609, #13567, #5106, #2059, #10614, #11638, #5017, #2949, #6472, #9626 ) ) ;
#4752 = ADVANCED_FACE ( 'NONE', ( #11445 ), #10299, .T. ) ;
#4753 = DIRECTION ( 'NONE',  ( 1.000000000000000000, 0.000000000000000000, 0.000000000000000000 ) ) ;
#4755 = EDGE_LOOP ( 'NONE', ( #431, #14640, #12547, #13584 ) ) ;
#4754 = CARTESIAN_POINT ( 'NONE',  ( -0.4124999999999999223, 0.1749999999999999889, 0.4124999999999999778 ) ) ;
#4756 = VERTEX_POINT ( 'NONE', #4415 ) ;
#4757 = LINE ( 'NONE', #7212, #911 ) ;
#4758 = DIRECTION ( 'NONE',  ( 0.000000000000000000, 0.000000000000000000, 1.000000000000000000 ) ) ;
#4759 = VERTEX_POINT ( 'NONE', #7852 ) ;
#4760 = CARTESIAN_POINT ( 'NONE',  ( -0.3725000000000000533, -0.6590000000000000302, 0.4424999999999981726 ) ) ;
#4761 = ADVANCED_FACE ( 'NONE', ( #12657 ), #2019, .T. ) ;
#4762 = VECTOR ( 'NONE', #13434, 39.37007874015748143 ) ;
#4763 = DIRECTION ( 'NONE',  ( 0.000000000000000000, -1.000000000000000000, 0.000000000000000000 ) ) ;
#4764 = CARTESIAN_POINT ( 'NONE',  ( 0.4349147617188414694, 1.239999999999999991, -0.008611041693277159473 ) ) ;
#4765 = VERTEX_POINT ( 'NONE', #14960 ) ;
#4766 = CARTESIAN_POINT ( 'NONE',  ( 0.7058998964907849949, -0.3829999999999992855, 0.4900296624789436950 ) ) ;
#4767 = DIRECTION ( 'NONE',  ( -0.000000000000000000, -1.000000000000000000, -0.000000000000000000 ) ) ;
#4768 = CARTESIAN_POINT ( 'NONE',  ( 3.875000000000000000, 1.059999999999999165, 0.5000000000000002220 ) ) ;
#4769 = ORIENTED_EDGE ( 'NONE', *, *, #12691, .F. ) ;
#4770 = DIRECTION ( 'NONE',  ( 0.000000000000000000, 0.000000000000000000, 1.000000000000000000 ) ) ;
#4771 = AXIS2_PLACEMENT_3D ( 'NONE', #7991, #2535, #14946 ) ;
#4772 = DIRECTION ( 'NONE',  ( 0.000000000000000000, 0.000000000000000000, -1.000000000000000000 ) ) ;
#4773 = ORIENTED_EDGE ( 'NONE', *, *, #14539, .T. ) ;
#4774 = CIRCLE ( 'NONE', #7228, 1.000000000000000222 ) ;
#4775 = AXIS2_PLACEMENT_3D ( 'NONE', #8849, #2808, #12136 ) ;
#4776 = DIRECTION ( 'NONE',  ( 0.000000000000000000, 0.000000000000000000, -1.000000000000000000 ) ) ;
#4777 = VERTEX_POINT ( 'NONE', #714 ) ;
#4778 = DIRECTION ( 'NONE',  ( 0.000000000000000000, 0.000000000000000000, -1.000000000000000000 ) ) ;
#4779 = LINE ( 'NONE', #9602, #13913 ) ;
#4780 = EDGE_CURVE ( 'NONE', #9554, #2583, #8249, .T. ) ;
#4781 = AXIS2_PLACEMENT_3D ( 'NONE', #9633, #14279, #5894 ) ;
#4782 = CARTESIAN_POINT ( 'NONE',  ( 6.176491571325181340, 0.000000000000000000, -2.960629921259842146 ) ) ;
#4783 = AXIS2_PLACEMENT_3D ( 'NONE', #13855, #4703, #7004 ) ;
#4784 = AXIS2_PLACEMENT_3D ( 'NONE', #5602, #4753, #11636 ) ;
#4785 = EDGE_CURVE ( 'NONE', #4697, #14026, #1625, .T. ) ;
#4786 = CARTESIAN_POINT ( 'NONE',  ( 0.000000000000000000, 0.04580000000000046534, -0.2499999999999999167 ) ) ;
#4787 = EDGE_LOOP ( 'NONE', ( #12800, #9284, #6358, #3094 ) ) ;
#4788 = ORIENTED_EDGE ( 'NONE', *, *, #6376, .T. ) ;
#4789 = EDGE_LOOP ( 'NONE', ( #14988, #10115, #10106, #10764 ) ) ;
#4790 = VECTOR ( 'NONE', #1607, 39.37007874015748143 ) ;
#4791 = FACE_BOUND ( 'NONE', #10377, .T. ) ;
#4792 = CARTESIAN_POINT ( 'NONE',  ( 3.426491571325181340, 2.426945040795776443, 0.5999481385559803925 ) ) ;
#4793 = AXIS2_PLACEMENT_3D ( 'NONE', #9378, #12723, #14101 ) ;
#4794 = AXIS2_PLACEMENT_3D ( 'NONE', #4125, #8003, #9075 ) ;
#4795 = DIRECTION ( 'NONE',  ( -0.000000000000000000, 1.000000000000000000, -0.000000000000000000 ) ) ;
#4796 = DIRECTION ( 'NONE',  ( 0.000000000000000000, 0.000000000000000000, 1.000000000000000000 ) ) ;
#4797 = LINE ( 'NONE', #8395, #13133 ) ;
#4798 = ORIENTED_EDGE ( 'NONE', *, *, #8710, .T. ) ;
#4799 = DIRECTION ( 'NONE',  ( -0.000000000000000000, -1.000000000000000000, 0.000000000000000000 ) ) ;
#4800 = CARTESIAN_POINT ( 'NONE',  ( 1.749262710669756693, 0.1141659463772449479, 0.4752928995668608270 ) ) ;
#4801 = CARTESIAN_POINT ( 'NONE',  ( 2.774999999999999911, -1.679378605318059048, -1.973878605318027724 ) ) ;
#4802 = ADVANCED_FACE ( 'NONE', ( #6868 ), #8259, .F. ) ;
#4803 = EDGE_CURVE ( 'NONE', #14441, #391, #13653, .T. ) ;
#4804 = AXIS2_PLACEMENT_3D ( 'NONE', #3451, #11788, #4911 ) ;
#4805 = AXIS2_PLACEMENT_3D ( 'NONE', #3319, #5393, #5624 ) ;
#4806 = CARTESIAN_POINT ( 'NONE',  ( -5.764454660286586870E-18, 0.1956296296296295978, -0.7406097974541305806 ) ) ;
#4807 = CARTESIAN_POINT ( 'NONE',  ( 4.575011402338617472, 1.741756125272902356, -0.2756533241654208211 ) ) ;
#4808 = EDGE_LOOP ( 'NONE', ( #10694, #7225, #12447, #10277 ) ) ;
#4810 = ORIENTED_EDGE ( 'NONE', *, *, #10945, .F. ) ;
#4809 = DIRECTION ( 'NONE',  ( 0.000000000000000000, 1.000000000000000000, 0.000000000000000000 ) ) ;
#4811 = EDGE_LOOP ( 'NONE', ( #13968, #8586 ) ) ;
#4812 = DIRECTION ( 'NONE',  ( 0.000000000000000000, -1.000000000000000000, 0.000000000000000000 ) ) ;
#4813 = ORIENTED_EDGE ( 'NONE', *, *, #13986, .T. ) ;
#4814 = DIRECTION ( 'NONE',  ( 0.000000000000000000, 0.000000000000000000, -1.000000000000000000 ) ) ;
#4815 = CIRCLE ( 'NONE', #2362, 0.2625000000000000111 ) ;
#4816 = SHAPE_DEFINITION_REPRESENTATION ( #643, #3685 ) ;
#4817 = DIRECTION ( 'NONE',  ( 0.000000000000000000, 0.000000000000000000, -1.000000000000000000 ) ) ;
#4818 = ORIENTED_EDGE ( 'NONE', *, *, #11847, .T. ) ;
#4819 = CARTESIAN_POINT ( 'NONE',  ( -0.03632416821535707635, 1.602793162442987418, -0.3809527529760087794 ) ) ;
#4820 = CARTESIAN_POINT ( 'NONE',  ( 2.774999999999999911, -2.359999999999984333, 1.575000000000016387 ) ) ;
#4821 = B_SPLINE_CURVE_WITH_KNOTS ( 'NONE', 3,
 ( #12753, #13822, #13745, #13974, #11622, #3285, #11704, #2281, #3510, #4360, #6891, #6964, #4436, #2124, #3360, #1046 ),
 .UNSPECIFIED., .F., .F.,
 ( 4, 2, 2, 2, 2, 2, 2, 4 ),
 ( 0.000000000000000000, 0.0005886476847306641811, 0.001177295369461328362, 0.001765943054191992543, 0.002354590738922656724, 0.002943238423653320689, 0.003531886108383985087, 0.004709181477845313449 ),
 .UNSPECIFIED. ) ;
#4822 = CARTESIAN_POINT ( 'NONE',  ( 3.618221289802627805, 1.960281491129935993, 0.7043865181403778930 ) ) ;
#4823 = AXIS2_PLACEMENT_3D ( 'NONE', #6257, #9771, #1715 ) ;
#4824 = EDGE_CURVE ( 'NONE', #13527, #14941, #8980, .T. ) ;
#4825 = FACE_OUTER_BOUND ( 'NONE', #13815, .T. ) ;
#4826 = CARTESIAN_POINT ( 'NONE',  ( 2.774999999999999911, 2.399999999999999911, -0.7000000000000009548 ) ) ;
#4827 = AXIS2_PLACEMENT_3D ( 'NONE', #13420, #13121, #6256 ) ;
#4828 = LINE ( 'NONE', #7052, #3399 ) ;
#4829 = FACE_OUTER_BOUND ( 'NONE', #5498, .T. ) ;
#4830 = EDGE_LOOP ( 'NONE', ( #11238, #12878, #8220, #5973 ) ) ;
#4831 = CARTESIAN_POINT ( 'NONE',  ( 0.6180000000000012150, 3.673940397442060361E-16, -3.000000000000000444 ) ) ;
#4833 = VERTEX_POINT ( 'NONE', #1868 ) ;
#4832 = DIRECTION ( 'NONE',  ( 0.000000000000000000, -1.000000000000000000, 0.000000000000000000 ) ) ;
#4834 = VERTEX_POINT ( 'NONE', #1021 ) ;
#4835 = AXIS2_PLACEMENT_3D ( 'NONE', #13899, #14831, #11544 ) ;
#4836 = DIRECTION ( 'NONE',  ( 0.000000000000000000, 0.000000000000000000, 1.000000000000000000 ) ) ;
#4837 = CARTESIAN_POINT ( 'NONE',  ( 0.8999999999999999112, -0.4829999999999998739, -0.3750000000000000555 ) ) ;
#4838 = DIRECTION ( 'NONE',  ( 0.000000000000000000, 0.000000000000000000, 1.000000000000000000 ) ) ;
#4839 = EDGE_LOOP ( 'NONE', ( #7972, #7119 ) ) ;
#4840 = DIRECTION ( 'NONE',  ( -1.000000000000000000, 0.000000000000000000, 0.000000000000000000 ) ) ;
#4841 = EDGE_CURVE ( 'NONE', #10348, #9682, #4186, .T. ) ;
#4842 = EDGE_CURVE ( 'NONE', #6905, #11355, #3258, .T. ) ;
#4843 = CARTESIAN_POINT ( 'NONE',  ( 0.6500000000000001332, 0.000000000000000000, 0.000000000000000000 ) ) ;
#4844 = EDGE_CURVE ( 'NONE', #5232, #6530, #6294, .T. ) ;
#4845 = CARTESIAN_POINT ( 'NONE',  ( 0.9717435313913082018, -0.4829764291992613701, -0.3975967162296610846 ) ) ;
#4846 = CIRCLE ( 'NONE', #6549, 0.06000000000000005329 ) ;
#4847 = ORIENTED_EDGE ( 'NONE', *, *, #12582, .F. ) ;
#4848 = CARTESIAN_POINT ( 'NONE',  ( 0.7204397385173402224, -0.4363855711863642850, 0.4582225808237245790 ) ) ;
#4849 = DIRECTION ( 'NONE',  ( 0.000000000000000000, -1.000000000000000000, 0.000000000000000000 ) ) ;
#4850 = DIRECTION ( 'NONE',  ( 1.000000000000000000, 0.000000000000000000, 0.000000000000000000 ) ) ;
#4851 = ORIENTED_EDGE ( 'NONE', *, *, #4841, .F. ) ;
#4852 = DIRECTION ( 'NONE',  ( -0.3420201433256621071, 0.000000000000000000, 0.9396926207859108704 ) ) ;
#4853 = EDGE_CURVE ( 'NONE', #7795, #9366, #6557, .T. ) ;
#4854 = CARTESIAN_POINT ( 'NONE',  ( 3.426491571325181340, -3.360000000000000320, 0.9799999999999999822 ) ) ;
#4855 = VERTEX_POINT ( 'NONE', #10075 ) ;
#4856 = AXIS2_PLACEMENT_3D ( 'NONE', #5011, #5861, #12875 ) ;
#4857 = LINE ( 'NONE', #12950, #13259 ) ;
#4858 = ORIENTED_EDGE ( 'NONE', *, *, #4803, .F. ) ;
#4859 = VECTOR ( 'NONE', #9332, 39.37007874015748143 ) ;
#4860 = LINE ( 'NONE', #1008, #10892 ) ;
#4861 = CARTESIAN_POINT ( 'NONE',  ( 0.9999999999999964473, -0.4429999999999999494, -0.4258697216429006005 ) ) ;
#4862 = EDGE_CURVE ( 'NONE', #11468, #4070, #12731, .T. ) ;
#4863 = AXIS2_PLACEMENT_3D ( 'NONE', #900, #5371, #4294 ) ;
#4864 = AXIS2_PLACEMENT_3D ( 'NONE', #494, #348, #6046 ) ;
#4865 = FACE_OUTER_BOUND ( 'NONE', #11160, .T. ) ;
#4866 = CONICAL_SURFACE ( 'NONE', #3874, 0.2624999999999997335, 0.7853981633974419507 ) ;
#4867 = DIRECTION ( 'NONE',  ( 0.000000000000000000, 1.000000000000000000, 0.000000000000000000 ) ) ;
#4868 = AXIS2_PLACEMENT_3D ( 'NONE', #14001, #4615, #3617 ) ;
#4869 = ORIENTED_EDGE ( 'NONE', *, *, #11050, .T. ) ;
#4870 = VERTEX_POINT ( 'NONE', #11289 ) ;
#4871 = VECTOR ( 'NONE', #4907, 39.37007874015748143 ) ;
#4872 = ORIENTED_EDGE ( 'NONE', *, *, #10706, .T. ) ;
#4873 = EDGE_CURVE ( 'NONE', #4452, #8991, #15111, .T. ) ;
#4874 = FACE_BOUND ( 'NONE', #12312, .T. ) ;
#4875 = CARTESIAN_POINT ( 'NONE',  ( 0.3753013551531362291, 1.599152118624413976, -0.1118644906773359898 ) ) ;
#4876 = FACE_OUTER_BOUND ( 'NONE', #5181, .T. ) ;
#4877 = VECTOR ( 'NONE', #5254, 39.37007874015748143 ) ;
#4878 = EDGE_CURVE ( 'NONE', #2583, #12064, #6628, .T. ) ;
#4879 = DIRECTION ( 'NONE',  ( 0.000000000000000000, -1.000000000000000000, 0.000000000000000000 ) ) ;
#4880 = ORIENTED_EDGE ( 'NONE', *, *, #12348, .F. ) ;
#4881 = AXIS2_PLACEMENT_3D ( 'NONE', #1722, #10156, #3036 ) ;
#4882 = CARTESIAN_POINT ( 'NONE',  ( 3.716581572976743075, 1.921374764163736426, -0.4747933410505347229 ) ) ;
#4883 = DIRECTION ( 'NONE',  ( -1.000000000000000000, -0.000000000000000000, -0.000000000000000000 ) ) ;
#4884 = CARTESIAN_POINT ( 'NONE',  ( -0.2849999999999996425, 0.000000000000000000, -0.4108223460329292753 ) ) ;
#4885 = AXIS2_PLACEMENT_3D ( 'NONE', #10452, #14321, #6224 ) ;
#4886 = CARTESIAN_POINT ( 'NONE',  ( 5.567023771132172172, 1.934941942652818220E-16, -1.580000000000000071 ) ) ;
#4887 = AXIS2_PLACEMENT_3D ( 'NONE', #2262, #7781, #6944 ) ;
#4888 = CARTESIAN_POINT ( 'NONE',  ( 2.088768908813758873, 0.2870784642939424591, -0.4704976142822916430 ) ) ;
#4889 = CARTESIAN_POINT ( 'NONE',  ( 4.466174989829828412, 1.785706766368954757, -0.4649126563571552295 ) ) ;
#4890 = ORIENTED_EDGE ( 'NONE', *, *, #7005, .T. ) ;
#4892 = ORIENTED_EDGE ( 'NONE', *, *, #12869, .T. ) ;
#4891 = CARTESIAN_POINT ( 'NONE',  ( 1.250847373107698779, -0.05999999999999997696, 0.4823326642216426707 ) ) ;
#4893 = VERTEX_POINT ( 'NONE', #13871 ) ;
#4894 = LINE ( 'NONE', #1119, #5544 ) ;
#4895 = ORIENTED_EDGE ( 'NONE', *, *, #2886, .T. ) ;
#4896 = EDGE_CURVE ( 'NONE', #4559, #4577, #5787, .T. ) ;
#4897 = DIRECTION ( 'NONE',  ( -0.000000000000000000, -1.000000000000000000, -0.000000000000000000 ) ) ;
#4898 = EDGE_CURVE ( 'NONE', #12744, #2839, #94, .T. ) ;
#4899 = DIRECTION ( 'NONE',  ( 0.000000000000000000, 1.000000000000000000, -0.000000000000000000 ) ) ;
#4900 = ORIENTED_EDGE ( 'NONE', *, *, #1769, .F. ) ;
#4901 = CARTESIAN_POINT ( 'NONE',  ( -0.1949587543783453114, 1.569534359386388411, -0.3809527529760086684 ) ) ;
#4902 = DIRECTION ( 'NONE',  ( 0.7071067811865429098, 8.659560562354987092E-17, 0.7071067811865521247 ) ) ;
#4903 = AXIS2_PLACEMENT_3D ( 'NONE', #12251, #5297, #12182 ) ;
#4904 = CARTESIAN_POINT ( 'NONE',  ( 3.562689364900068156, 1.987812937981572770, 0.6814576478706133589 ) ) ;
#4905 = CARTESIAN_POINT ( 'NONE',  ( 8.524379033352621704, 0.9303642257649958891, 0.3795991661955845919 ) ) ;
#4906 = DIRECTION ( 'NONE',  ( 1.000000000000000000, 0.000000000000000000, 0.000000000000000000 ) ) ;
#4907 = DIRECTION ( 'NONE',  ( -1.000000000000000000, -0.000000000000000000, -0.000000000000000000 ) ) ;
#4908 = CARTESIAN_POINT ( 'NONE',  ( 4.618921047797687862, 1.723044742589275646, -0.3137129605234482699 ) ) ;
#4909 = EDGE_LOOP ( 'NONE', ( #374, #13194, #13647, #14171 ) ) ;
#4910 = CARTESIAN_POINT ( 'NONE',  ( 0.6555107925675723868, -0.4029228396118701983, 0.5098556521091195393 ) ) ;
#4912 = EDGE_LOOP ( 'NONE', ( #12617, #8905 ) ) ;
#4911 = DIRECTION ( 'NONE',  ( 0.000000000000000000, 0.000000000000000000, 1.000000000000000000 ) ) ;
#4913 = VERTEX_POINT ( 'NONE', #9466 ) ;
#4914 = LINE ( 'NONE', #14155, #14357 ) ;
#4915 = ADVANCED_FACE ( 'NONE', ( #14110 ), #10527, .F. ) ;
#4916 =( NAMED_UNIT ( * ) SI_UNIT ( $, .STERADIAN. ) SOLID_ANGLE_UNIT ( ) );
#4917 = CARTESIAN_POINT ( 'NONE',  ( 3.320735777595773541, 0.6889667851711056556, 0.4530969522938014249 ) ) ;
#4918 = ORIENTED_EDGE ( 'NONE', *, *, #4476, .F. ) ;
#4919 = CARTESIAN_POINT ( 'NONE',  ( 1.537522204129377457, -0.4429999999999995053, 0.4185053637614668531 ) ) ;
#4920 = CARTESIAN_POINT ( 'NONE',  ( 6.176491571325181340, -1.679378605318048390, 1.679378605318054163 ) ) ;
#4921 = LINE ( 'NONE', #8514, #12666 ) ;
#4922 = EDGE_LOOP ( 'NONE', ( #4980, #2118, #10802, #10525 ) ) ;
#4923 = LINE ( 'NONE', #9591, #12533 ) ;
#4924 = DIRECTION ( 'NONE',  ( 0.000000000000000000, -1.000000000000000000, 0.000000000000000000 ) ) ;
#4925 = DIRECTION ( 'NONE',  ( -0.000000000000000000, 1.836536466328828134E-14, 1.000000000000000000 ) ) ;
#4926 = CARTESIAN_POINT ( 'NONE',  ( 2.124999999999999556, -3.360000000000000320, 0.9799999999999999822 ) ) ;
#4927 = ORIENTED_EDGE ( 'NONE', *, *, #4519, .F. ) ;
#4928 = FACE_OUTER_BOUND ( 'NONE', #1114, .T. ) ;
#4929 = CONICAL_SURFACE ( 'NONE', #12235, 0.2944999999999987073, 0.7853981633974366217 ) ;
#4930 = CARTESIAN_POINT ( 'NONE',  ( 3.875000000000000000, 3.085321731235734610, -0.5849999999999996314 ) ) ;
#4931 = VERTEX_POINT ( 'NONE', #12806 ) ;
#4932 = EDGE_CURVE ( 'NONE', #15129, #4391, #8394, .T. ) ;
#4933 = CARTESIAN_POINT ( 'NONE',  ( -0.3390120837646902197, 1.603403006623433491, 0.1747193524917784735 ) ) ;
#4934 = VERTEX_POINT ( 'NONE', #6940 ) ;
#4935 = DIRECTION ( 'NONE',  ( -0.7070715176384863021, -0.7070715176384774203, 0.009986885842351498482 ) ) ;
#4936 = CARTESIAN_POINT ( 'NONE',  ( 1.860560713452861892, -0.1867359432425545751, -0.4737208938777845435 ) ) ;
#4937 = DIRECTION ( 'NONE',  ( -0.000000000000000000, 1.000000000000000000, 0.000000000000000000 ) ) ;
#4938 = CONICAL_SURFACE ( 'NONE', #8100, 0.3750000000000004996, 0.7853981633974547183 ) ;
#4939 = DIRECTION ( 'NONE',  ( 0.000000000000000000, 0.000000000000000000, 1.000000000000000000 ) ) ;
#4940 = CARTESIAN_POINT ( 'NONE',  ( 3.875000000000000000, 1.059999999999999165, 0.5000000000000002220 ) ) ;
#4941 = ORIENTED_EDGE ( 'NONE', *, *, #5816, .T. ) ;
#4942 = ORIENTED_EDGE ( 'NONE', *, *, #15130, .T. ) ;
#4943 = EDGE_CURVE ( 'NONE', #3132, #5891, #11080, .T. ) ;
#4944 = ORIENTED_EDGE ( 'NONE', *, *, #7673, .T. ) ;
#4945 = ADVANCED_FACE ( 'NONE', ( #9389 ), #14028, .F. ) ;
#4946 = DIRECTION ( 'NONE',  ( -1.000000000000000000, -0.000000000000000000, -0.000000000000000000 ) ) ;
#4947 = EDGE_CURVE ( 'NONE', #8178, #11602, #4564, .T. ) ;
#4948 = MECHANICAL_DESIGN_GEOMETRIC_PRESENTATION_REPRESENTATION (  '', ( #6158 ), #6166 ) ;
#4949 = CARTESIAN_POINT ( 'NONE',  ( 8.475037399843312613, 0.9969999999999998863, -0.3802960819231170908 ) ) ;
#4950 = DIRECTION ( 'NONE',  ( -1.000000000000000000, -0.000000000000000000, -0.000000000000000000 ) ) ;
#4951 = DIRECTION ( 'NONE',  ( -1.000000000000000000, -0.000000000000000000, -0.000000000000000000 ) ) ;
#4952 = PRODUCT_DEFINITION_SHAPE ( 'NONE', 'NONE',  #15157 ) ;
#4953 = ORIENTED_EDGE ( 'NONE', *, *, #2397, .T. ) ;
#4954 = CARTESIAN_POINT ( 'NONE',  ( 3.473767154576092864, 1.977251034363303628, -0.3019842868889652809 ) ) ;
#4955 = EDGE_CURVE ( 'NONE', #628, #8247, #6902, .T. ) ;
#4956 = DIRECTION ( 'NONE',  ( -0.7071067811865519026, -0.7071067811865430208, 0.000000000000000000 ) ) ;
#4957 = SURFACE_STYLE_USAGE ( .BOTH. , #3002 ) ;
#4958 = ADVANCED_FACE ( 'NONE', ( #4876 ), #10681, .F. ) ;
#4959 = DIRECTION ( 'NONE',  ( -1.000000000000000000, -0.000000000000000000, -0.000000000000000000 ) ) ;
#4960 = EDGE_LOOP ( 'NONE', ( #10575, #13359, #2770, #3541 ) ) ;
#4962 = ORIENTED_EDGE ( 'NONE', *, *, #4700, .F. ) ;
#4961 = DIRECTION ( 'NONE',  ( 0.000000000000000000, 0.000000000000000000, -1.000000000000000000 ) ) ;
#4963 = ORIENTED_EDGE ( 'NONE', *, *, #1950, .F. ) ;
#4964 = PLANE ( 'NONE',  #6776 ) ;
#4965 = VERTEX_POINT ( 'NONE', #13952 ) ;
#4966 = VECTOR ( 'NONE', #8142, 39.37007874015748143 ) ;
#4967 = PRODUCT_CONTEXT ( 'NONE', #6078, 'mechanical' ) ;
#4968 = CYLINDRICAL_SURFACE ( 'NONE', #4781, 1.000000000000000222 ) ;
#4969 = ORIENTED_EDGE ( 'NONE', *, *, #4955, .T. ) ;
#4970 = DIRECTION ( 'NONE',  ( 0.000000000000000000, 0.000000000000000000, -1.000000000000000000 ) ) ;
#4971 = LINE ( 'NONE', #9705, #4622 ) ;
#4972 = EDGE_CURVE ( 'NONE', #9226, #5697, #9232, .T. ) ;
#4973 = CARTESIAN_POINT ( 'NONE',  ( 2.980731298636167370, 3.567999999999999616, 0.3249191361593796734 ) ) ;
#4974 = EDGE_CURVE ( 'NONE', #5730, #9564, #13950, .T. ) ;
#4975 = FACE_OUTER_BOUND ( 'NONE', #7150, .T. ) ;
#4976 = CARTESIAN_POINT ( 'NONE',  ( 0.8310910854522474134, -0.4382321058747689624, -0.4519764243385314129 ) ) ;
#4977 = EDGE_CURVE ( 'NONE', #4021, #557, #3792, .T. ) ;
#4978 = CARTESIAN_POINT ( 'NONE',  ( 3.659655290762535262, 1.940877740142120222, 0.7181426529861060226 ) ) ;
#4979 = DIRECTION ( 'NONE',  ( 0.000000000000000000, 0.000000000000000000, -1.000000000000000000 ) ) ;
#4980 = ORIENTED_EDGE ( 'NONE', *, *, #2452, .F. ) ;
#4981 = AXIS2_PLACEMENT_3D ( 'NONE', #11985, #13040, #12257 ) ;
#4982 = DIRECTION ( 'NONE',  ( -1.000000000000000000, -0.000000000000000000, -0.000000000000000000 ) ) ;
#4984 = ORIENTED_EDGE ( 'NONE', *, *, #4280, .F. ) ;
#4983 = CYLINDRICAL_SURFACE ( 'NONE', #2596, 0.07500000000000002498 ) ;
#4985 = ORIENTED_EDGE ( 'NONE', *, *, #8353, .F. ) ;
#4986 = AXIS2_PLACEMENT_3D ( 'NONE', #9600, #455, #10811 ) ;
#4987 = CARTESIAN_POINT ( 'NONE',  ( 0.4125000000000000333, 0.000000000000000000, 0.3724999999999999978 ) ) ;
#4988 = CARTESIAN_POINT ( 'NONE',  ( 0.6601485485260571995, -0.07064835164835162051, -0.5137583810202324131 ) ) ;
#4989 = DIRECTION ( 'NONE',  ( 1.000000000000000000, 0.000000000000000000, 0.000000000000000000 ) ) ;
#4990 = ORIENTED_EDGE ( 'NONE', *, *, #14852, .F. ) ;
#4991 = FACE_OUTER_BOUND ( 'NONE', #6471, .T. ) ;
#4992 = CARTESIAN_POINT ( 'NONE',  ( 0.6746193685512165139, -0.05586318815840191770, 0.4906972545532043428 ) ) ;
#4993 = AXIS2_PLACEMENT_3D ( 'NONE', #13205, #11998, #1507 ) ;
#4994 = DIRECTION ( 'NONE',  ( 0.000000000000000000, 0.000000000000000000, -1.000000000000000000 ) ) ;
#4995 = AXIS2_PLACEMENT_3D ( 'NONE', #8131, #5911, #2142 ) ;
#4996 = VERTEX_POINT ( 'NONE', #10904 ) ;
#4997 = EDGE_CURVE ( 'NONE', #539, #969, #1250, .T. ) ;
#4998 = DIRECTION ( 'NONE',  ( 0.000000000000000000, 0.000000000000000000, -1.000000000000000000 ) ) ;
#4999 = CARTESIAN_POINT ( 'NONE',  ( 1.539501593423603154, -0.4421672100983570219, -0.4184782450098369910 ) ) ;
#5000 = LINE ( 'NONE', #370, #3000 ) ;
#5001 = CARTESIAN_POINT ( 'NONE',  ( 2.806999999999999940, -1.679378605318059048, -1.679378605318041950 ) ) ;
#5002 = VERTEX_POINT ( 'NONE', #5094 ) ;
#5003 = LINE ( 'NONE', #5995, #14435 ) ;
#5004 = CARTESIAN_POINT ( 'NONE',  ( 2.187203820042824542, 0.4712135623730921985, 0.4085020630706684974 ) ) ;
#5005 = EDGE_LOOP ( 'NONE', ( #8660, #3629, #6515, #3916 ) ) ;
#5006 = CARTESIAN_POINT ( 'NONE',  ( -0.3662167046613059029, 1.600826314462298061, 0.1275995668981904640 ) ) ;
#5007 =( REPRESENTATION_RELATIONSHIP ('NONE','NONE', #3591, #3685 ) REPRESENTATION_RELATIONSHIP_WITH_TRANSFORMATION ( #6405 )SHAPE_REPRESENTATION_RELATIONSHIP( ) );
#5008 = ORIENTED_EDGE ( 'NONE', *, *, #11686, .T. ) ;
#5009 = VECTOR ( 'NONE', #11481, 39.37007874015748143 ) ;
#5010 = LINE ( 'NONE', #7444, #11732 ) ;
#5011 = CARTESIAN_POINT ( 'NONE',  ( 2.774999999999999911, 0.000000000000000000, 0.000000000000000000 ) ) ;
#5012 = CARTESIAN_POINT ( 'NONE',  ( 0.09500000000000431710, -1.679378605318047946, -1.304378605318053053 ) ) ;
#5013 = CIRCLE ( 'NONE', #7447, 0.05999999999999990757 ) ;
#5014 = CARTESIAN_POINT ( 'NONE',  ( 3.874999999999999556, 3.137999999999999901, -1.320000000000000062 ) ) ;
#5015 = EDGE_CURVE ( 'NONE', #7227, #7182, #13408, .T. ) ;
#5016 = EDGE_LOOP ( 'NONE', ( #5463, #737, #118, #4463 ) ) ;
#5017 = ORIENTED_EDGE ( 'NONE', *, *, #13478, .T. ) ;
#5018 = ORIENTED_EDGE ( 'NONE', *, *, #4651, .F. ) ;
#5019 = FACE_OUTER_BOUND ( 'NONE', #11828, .T. ) ;
#5020 = DIRECTION ( 'NONE',  ( -1.000000000000000000, -0.000000000000000000, -0.000000000000000000 ) ) ;
#5021 = DIRECTION ( 'NONE',  ( 0.000000000000000000, 0.000000000000000000, 1.000000000000000000 ) ) ;
#5022 = AXIS2_PLACEMENT_3D ( 'NONE', #13674, #15059, #13591 ) ;
#5023 = FACE_OUTER_BOUND ( 'NONE', #8009, .T. ) ;
#5024 = CARTESIAN_POINT ( 'NONE',  ( 3.875000000000000000, 3.137999999999999901, 0.000000000000000000 ) ) ;
#5025 = VECTOR ( 'NONE', #3090, 39.37007874015748143 ) ;
#5026 = AXIS2_PLACEMENT_3D ( 'NONE', #4843, #6141, #10728 ) ;
#5027 = CARTESIAN_POINT ( 'NONE',  ( 1.405961592616383316, -0.05236138586009463081, 0.4801417854150228370 ) ) ;
#5028 = EDGE_CURVE ( 'NONE', #1342, #5706, #10308, .T. ) ;
#5029 = EDGE_CURVE ( 'NONE', #11113, #10200, #510, .T. ) ;
#5030 = EDGE_CURVE ( 'NONE', #2008, #2639, #13466, .T. ) ;
#5031 = AXIS2_PLACEMENT_3D ( 'NONE', #9808, #14699, #14461 ) ;
#5032 = VERTEX_POINT ( 'NONE', #11978 ) ;
#5034 = VERTEX_POINT ( 'NONE', #8679 ) ;
#5033 = FACE_OUTER_BOUND ( 'NONE', #10319, .T. ) ;
#5035 = CONICAL_SURFACE ( 'NONE', #597, 0.4070000000000022489, 0.7853981633974547183 ) ;
#5036 = ADVANCED_FACE ( 'NONE', ( #9905 ), #2645, .T. ) ;
#5037 = ORIENTED_EDGE ( 'NONE', *, *, #10175, .T. ) ;
#5038 = LINE ( 'NONE', #9697, #12624 ) ;
#5039 = DIRECTION ( 'NONE',  ( 0.000000000000000000, 1.000000000000000000, 0.000000000000000000 ) ) ;
#5040 = CARTESIAN_POINT ( 'NONE',  ( 4.167248288244303822, 0.9139185452513080010, 0.4060177403750064307 ) ) ;
#5041 = SHAPE_DEFINITION_REPRESENTATION ( #2867, #3591 ) ;
#5042 = CARTESIAN_POINT ( 'NONE',  ( 3.426491571325181340, 1.575000000000016387, 2.359999999999999876 ) ) ;
#5043 = ORIENTED_EDGE ( 'NONE', *, *, #5649, .T. ) ;
#5044 = CYLINDRICAL_SURFACE ( 'NONE', #4344, 3.000000000000000444 ) ;
#5045 = DIRECTION ( 'NONE',  ( -1.000000000000000000, -0.000000000000000000, -0.000000000000000000 ) ) ;
#5046 = AXIS2_PLACEMENT_3D ( 'NONE', #14152, #12996, #9426 ) ;
#5047 = DIRECTION ( 'NONE',  ( 0.000000000000000000, 0.000000000000000000, 1.000000000000000000 ) ) ;
#5048 = AXIS2_PLACEMENT_3D ( 'NONE', #13058, #12147, #10628 ) ;
#5049 = VECTOR ( 'NONE', #4561, 39.37007874015748854 ) ;
#5050 = CARTESIAN_POINT ( 'NONE',  ( 3.874999999999999556, 3.137999999999999901, -1.320000000000000062 ) ) ;
#5051 = DIRECTION ( 'NONE',  ( 0.000000000000000000, 0.000000000000000000, -1.000000000000000000 ) ) ;
#5052 = CARTESIAN_POINT ( 'NONE',  ( 3.740430787191658446, 1.905565248334865736, 0.7383113636965974447 ) ) ;
#5053 = CARTESIAN_POINT ( 'NONE',  ( 2.001999999999999780, 1.653273178848927113E-16, -1.350000000000000089 ) ) ;
#5054 = CIRCLE ( 'NONE', #7988, 0.4999999999999997224 ) ;
#5055 = EDGE_LOOP ( 'NONE', ( #8111, #8265 ) ) ;
#5056 = DIRECTION ( 'NONE',  ( -1.655665450705613915E-16, -3.103226861728128995E-32, -1.000000000000000000 ) ) ;
#5058 = ORIENTED_EDGE ( 'NONE', *, *, #5994, .F. ) ;
#5057 = CARTESIAN_POINT ( 'NONE',  ( 3.426491571325181340, 1.575000000000016609, 1.575000000000000178 ) ) ;
#5059 = VERTEX_POINT ( 'NONE', #3944 ) ;
#5060 = ADVANCED_FACE ( 'NONE', ( #7605 ), #270, .T. ) ;
#5061 = CARTESIAN_POINT ( 'NONE',  ( 0.6940366006580476199, 0.04143956043956066593, 0.4146323121508169729 ) ) ;
#5062 = CARTESIAN_POINT ( 'NONE',  ( 0.000000000000000000, 0.000000000000000000, 0.000000000000000000 ) ) ;
#5063 = CARTESIAN_POINT ( 'NONE',  ( 3.875000000000000000, 3.567999999999999616, 0.000000000000000000 ) ) ;
#5064 = ORIENTED_EDGE ( 'NONE', *, *, #2502, .F. ) ;
#5065 = CYLINDRICAL_SURFACE ( 'NONE', #1421, 1.000000000000000000 ) ;
#5066 = EDGE_CURVE ( 'NONE', #1274, #13460, #4694, .T. ) ;
#5067 = VECTOR ( 'NONE', #13338, 39.37007874015748143 ) ;
#5068 = CARTESIAN_POINT ( 'NONE',  ( 0.7145271609291293791, -0.01099779881553469840, 0.4647412378891488394 ) ) ;
#5069 = CARTESIAN_POINT ( 'NONE',  ( 3.426491571325181340, 2.449513323269931135E-16, -2.000179419058113695 ) ) ;
#5070 = ORIENTED_EDGE ( 'NONE', *, *, #3723, .F. ) ;
#5071 = DIRECTION ( 'NONE',  ( 0.000000000000000000, 0.000000000000000000, -1.000000000000000000 ) ) ;
#5072 = VECTOR ( 'NONE', #13124, 39.37007874015748143 ) ;
#5073 = CARTESIAN_POINT ( 'NONE',  ( 0.06299999999999998657, 2.296825071800860970E-16, 1.875500000000000167 ) ) ;
#5074 = CARTESIAN_POINT ( 'NONE',  ( -0.3724999999999999423, 0.1749999999999999889, 0.3724999999999999978 ) ) ;
#5075 = VERTEX_POINT ( 'NONE', #2722 ) ;
#5076 = DIRECTION ( 'NONE',  ( -0.000000000000000000, -1.000000000000000000, -0.000000000000000000 ) ) ;
#5077 = ORIENTED_EDGE ( 'NONE', *, *, #14038, .T. ) ;
#5078 = CARTESIAN_POINT ( 'NONE',  ( 2.045495128834867060, 0.3295048711651353268, 0.4105035982572216025 ) ) ;
#5079 = EDGE_LOOP ( 'NONE', ( #14353, #3032, #10143, #3089 ) ) ;
#5080 = FILL_AREA_STYLE_COLOUR ( '', #14880 ) ;
#5081 = EDGE_CURVE ( 'NONE', #7714, #14724, #10798, .T. ) ;
#5082 = CARTESIAN_POINT ( 'NONE',  ( 2.980731298636167370, 3.567999999999999616, -0.3249191361593797844 ) ) ;
#5083 = AXIS2_PLACEMENT_3D ( 'NONE', #9704, #9776, #1795 ) ;
#5084 = CARTESIAN_POINT ( 'NONE',  ( 0.7893200925859867878, -0.4447764794942862809, -0.3170959440181289613 ) ) ;
#5085 = DIRECTION ( 'NONE',  ( 0.000000000000000000, 0.000000000000000000, -1.000000000000000000 ) ) ;
#5086 = DIRECTION ( 'NONE',  ( -1.000000000000000000, -0.000000000000000000, -0.000000000000000000 ) ) ;
#5087 = AXIS2_PLACEMENT_3D ( 'NONE', #4406, #6625, #774 ) ;
#5088 = VERTEX_POINT ( 'NONE', #315 ) ;
#5089 = ORIENTED_EDGE ( 'NONE', *, *, #5239, .F. ) ;
#5090 = VECTOR ( 'NONE', #13071, 39.37007874015748143 ) ;
#5091 = ORIENTED_EDGE ( 'NONE', *, *, #10479, .F. ) ;
#5092 = CARTESIAN_POINT ( 'NONE',  ( 2.230049639690012242, 0.4283591951701958278, -0.4685021237331919441 ) ) ;
#5093 = DIRECTION ( 'NONE',  ( -1.000000000000000000, -0.000000000000000000, -0.000000000000000000 ) ) ;
#5094 = CARTESIAN_POINT ( 'NONE',  ( 2.774999999999999911, 1.679378605318042395, -1.973878605318059698 ) ) ;
#5095 = DIRECTION ( 'NONE',  ( 0.000000000000000000, 1.000000000000000000, 0.000000000000000000 ) ) ;
#5096 = CIRCLE ( 'NONE', #11188, 0.4070000000000022489 ) ;
#5097 = CARTESIAN_POINT ( 'NONE',  ( 3.426491571325181340, 1.986447008166981387, -0.6339330177794473276 ) ) ;
#5098 = CARTESIAN_POINT ( 'NONE',  ( 2.807000000000000384, 1.679378605318059048, 1.941878605318041462 ) ) ;
#5099 = VECTOR ( 'NONE', #3978, 39.37007874015748854 ) ;
#5100 = DIRECTION ( 'NONE',  ( 0.000000000000000000, 1.000000000000000000, 0.000000000000000000 ) ) ;
#5101 =( NAMED_UNIT ( * ) SI_UNIT ( $, .STERADIAN. ) SOLID_ANGLE_UNIT ( ) );
#5102 = FACE_OUTER_BOUND ( 'NONE', #4830, .T. ) ;
#5103 = CIRCLE ( 'NONE', #669, 0.3750000000000004996 ) ;
#5104 = VECTOR ( 'NONE', #3984, 39.37007874015748143 ) ;
#5105 = CIRCLE ( 'NONE', #14378, 0.3750000000000004996 ) ;
#5106 = ORIENTED_EDGE ( 'NONE', *, *, #14078, .T. ) ;
#5107 = EDGE_LOOP ( 'NONE', ( #10858, #11620 ) ) ;
#5108 = AXIS2_PLACEMENT_3D ( 'NONE', #11849, #11921, #13130 ) ;
#5109 = CIRCLE ( 'NONE', #14634, 0.4070000000000058016 ) ;
#5110 = VERTEX_POINT ( 'NONE', #7393 ) ;
#5111 = LINE ( 'NONE', #4025, #5067 ) ;
#5112 = EDGE_CURVE ( 'NONE', #6694, #754, #12046, .T. ) ;
#5113 = FACE_OUTER_BOUND ( 'NONE', #7701, .T. ) ;
#5114 = CARTESIAN_POINT ( 'NONE',  ( 3.875000000000000000, 0.8660254037844384856, 0.5000000000000002220 ) ) ;
#5115 = LENGTH_MEASURE_WITH_UNIT ( LENGTH_MEASURE( 0.02539999999999999897 ), #9701 );
#5116 = DIRECTION ( 'NONE',  ( -1.000000000000000000, -0.000000000000000000, -0.000000000000000000 ) ) ;
#5117 = ORIENTED_EDGE ( 'NONE', *, *, #3639, .F. ) ;
#5118 = AXIS2_PLACEMENT_3D ( 'NONE', #14454, #2762, #6213 ) ;
#5119 = LINE ( 'NONE', #3961, #13846 ) ;
#5120 = DIRECTION ( 'NONE',  ( -0.9992912762382412106, -0.03489602031262427351, -0.01411428356269072044 ) ) ;
#5121 = LINE ( 'NONE', #13204, #2695 ) ;
#5122 = VECTOR ( 'NONE', #13953, 39.37007874015748143 ) ;
#5123 = AXIS2_PLACEMENT_3D ( 'NONE', #14948, #10063, #11347 ) ;
#5124 = EDGE_CURVE ( 'NONE', #5889, #2080, #11780, .T. ) ;
#5125 = CARTESIAN_POINT ( 'NONE',  ( 3.875000000000000000, 1.059999999999999165, -0.5000000000000002220 ) ) ;
#5126 = CARTESIAN_POINT ( 'NONE',  ( 2.124999999999999556, 3.360000000000000320, -0.9800000000000012035 ) ) ;
#5127 = CARTESIAN_POINT ( 'NONE',  ( 3.841433886848298673, 1.867524044941962558, 0.7493717214423840645 ) ) ;
#5128 = CYLINDRICAL_SURFACE ( 'NONE', #3532, 0.2624999999999997335 ) ;
#5129 = ORIENTED_EDGE ( 'NONE', *, *, #14819, .F. ) ;
#5130 = DIRECTION ( 'NONE',  ( 0.000000000000000000, 1.000000000000000000, 0.000000000000000000 ) ) ;
#5131 = ORIENTED_EDGE ( 'NONE', *, *, #144, .T. ) ;
#5132 = EDGE_LOOP ( 'NONE', ( #9411, #6962, #5593, #5426 ) ) ;
#5133 = EDGE_CURVE ( 'NONE', #12982, #863, #11034, .T. ) ;
#5134 = AXIS2_PLACEMENT_3D ( 'NONE', #6082, #9303, #10748 ) ;
#5135 = LINE ( 'NONE', #506, #10217 ) ;
#5136 = SHAPE_REPRESENTATION_RELATIONSHIP ( 'NONE' , 'NONE' ,  #10912, #14565 ) ;
#5137 = CARTESIAN_POINT ( 'NONE',  ( 2.806999999999999496, -1.679378605318041950, 1.679378605318059048 ) ) ;
#5138 = ORIENTED_EDGE ( 'NONE', *, *, #7506, .T. ) ;
#5139 = EDGE_CURVE ( 'NONE', #13964, #10623, #487, .T. ) ;
#5140 = CARTESIAN_POINT ( 'NONE',  ( 0.2099999999999999922, 0.7512260236060024354, 0.3809527529760087239 ) ) ;
#5141 = EDGE_CURVE ( 'NONE', #12434, #13095, #13326, .T. ) ;
#5142 = CARTESIAN_POINT ( 'NONE',  ( 0.7010312871322611494, 0.003350962741495644263, 0.4267273516602812511 ) ) ;
#5143 = CARTESIAN_POINT ( 'NONE',  ( -0.4124999999999999223, 0.1749999999999999889, -0.3724999999999999978 ) ) ;
#5144 = ADVANCED_FACE ( 'NONE', ( #5548 ), #1779, .T. ) ;
#5145 = AXIS2_PLACEMENT_3D ( 'NONE', #15143, #755, #11260 ) ;
#5146 = EDGE_LOOP ( 'NONE', ( #7681, #6214, #3788, #6655, #6802 ) ) ;
#5147 = CARTESIAN_POINT ( 'NONE',  ( 3.875000000000000000, 3.567999999999999616, 0.4849999999999995981 ) ) ;
#5148 = PLANE ( 'NONE',  #7632 ) ;
#5149 = CARTESIAN_POINT ( 'NONE',  ( 0.000000000000000000, 0.000000000000000000, 1.350000000000000089 ) ) ;
#5150 = FACE_OUTER_BOUND ( 'NONE', #4349, .T. ) ;
#5151 = VERTEX_POINT ( 'NONE', #3099 ) ;
#5152 = CARTESIAN_POINT ( 'NONE',  ( -0.3753013551531455549, 1.599152118624412644, 0.1118644906773185593 ) ) ;
#5153 = ORIENTED_EDGE ( 'NONE', *, *, #4405, .T. ) ;
#5154 = CARTESIAN_POINT ( 'NONE',  ( 6.096491571325181269, 0.000000000000000000, 0.000000000000000000 ) ) ;
#5155 = EDGE_CURVE ( 'NONE', #13458, #10542, #3951, .T. ) ;
#5156 = CARTESIAN_POINT ( 'NONE',  ( 0.8258103947154198377, -0.4830000013490253208, -0.3634202042301618585 ) ) ;
#5157 = CARTESIAN_POINT ( 'NONE',  ( 3.875000000000000000, 0.7099999999999984102, 0.000000000000000000 ) ) ;
#5158 = CARTESIAN_POINT ( 'NONE',  ( 2.774999999999999911, 0.9800000000000039790, 3.360000000000000320 ) ) ;
#5159 = AXIS2_PLACEMENT_3D ( 'NONE', #6023, #10686, #5383 ) ;
#5160 = CARTESIAN_POINT ( 'NONE',  ( 1.936238515863220711, 0.2305039212133961901, -0.4121290732901491949 ) ) ;
#5161 = EDGE_CURVE ( 'NONE', #11971, #9822, #11120, .T. ) ;
#5162 = VERTEX_POINT ( 'NONE', #1857 ) ;
#5163 = ORIENTED_EDGE ( 'NONE', *, *, #2706, .F. ) ;
#5164 = ORIENTED_EDGE ( 'NONE', *, *, #42, .F. ) ;
#5165 = CARTESIAN_POINT ( 'NONE',  ( 0.3724999999999999423, -0.6590000000000000302, 0.3724999999999999423 ) ) ;
#5166 = LINE ( 'NONE', #2567, #11665 ) ;
#5167 = DIRECTION ( 'NONE',  ( 0.000000000000000000, 0.000000000000000000, -1.000000000000000000 ) ) ;
#5168 = CARTESIAN_POINT ( 'NONE',  ( 6.826491571325181695, -1.679378605318048390, 1.679378605318054163 ) ) ;
#5169 = CARTESIAN_POINT ( 'NONE',  ( 6.794491571325179891, -1.679378605318048390, 1.679378605318054163 ) ) ;
#5170 = CARTESIAN_POINT ( 'NONE',  ( 4.512545870194937692, 1.791067049260529176, -0.3982799620645194882 ) ) ;
#5171 = DIRECTION ( 'NONE',  ( 1.000000000000000000, 0.000000000000000000, 0.000000000000000000 ) ) ;
#5172 = ADVANCED_FACE ( 'NONE', ( #7761 ), #6690, .F. ) ;
#5173 = CONICAL_SURFACE ( 'NONE', #9593, 0.2944999999999845519, 0.7853981633974509435 ) ;
#5174 = ORIENTED_EDGE ( 'NONE', *, *, #6805, .T. ) ;
#5175 = ORIENTED_EDGE ( 'NONE', *, *, #14705, .F. ) ;
#5176 = ORIENTED_EDGE ( 'NONE', *, *, #7782, .F. ) ;
#5177 = CARTESIAN_POINT ( 'NONE',  ( 0.1786439721334352748, 1.577722767886655886, 0.3809527529760086684 ) ) ;
#5178 = CARTESIAN_POINT ( 'NONE',  ( 0.8999999999999999112, -0.4829999999999998739, -0.3750000000000000555 ) ) ;
#5179 = CARTESIAN_POINT ( 'NONE',  ( 2.124999999999999556, 0.6999999999999599876, -2.400000000000011458 ) ) ;
#5180 = CARTESIAN_POINT ( 'NONE',  ( 0.8254245316410396827, -0.4829999999999998739, -0.3670313414528085239 ) ) ;
#5181 = EDGE_LOOP ( 'NONE', ( #7139, #3726, #3643, #7730 ) ) ;
#5182 = CARTESIAN_POINT ( 'NONE',  ( 6.794491571325179891, -1.679378605318048390, 1.679378605318054163 ) ) ;
#5183 = FACE_OUTER_BOUND ( 'NONE', #12998, .T. ) ;
#5184 = CARTESIAN_POINT ( 'NONE',  ( 0.6179999999999965521, 1.679378605318059492, 2.054378605318042172 ) ) ;
#5185 = PRODUCT ( 'Outlet Housing', 'Outlet Housing', '', ( #9773 ) ) ;
#5186 = CARTESIAN_POINT ( 'NONE',  ( 8.752374375191447342, 0.8785908380595733869, 0.1599881670920847154 ) ) ;
#5187 = CARTESIAN_POINT ( 'NONE',  ( 0.8482706842831971850, -0.4349723313396169910, -0.4582157225860795102 ) ) ;
#5188 = CARTESIAN_POINT ( 'NONE',  ( 2.774999999999999911, -1.679378605318041950, 1.679378605318059048 ) ) ;
#5189 = PRODUCT_RELATED_PRODUCT_CATEGORY ( 'part', '', ( #12267 ) ) ;
#5190 = CARTESIAN_POINT ( 'NONE',  ( 3.495307681290304114, 1.921430432632648122, 0.7213508312486736074 ) ) ;
#5192 = EDGE_LOOP ( 'NONE', ( #1141, #8180, #8712, #6731, #6701, #8674, #11970, #13493, #804, #6143, #14292, #6428, #9964, #8846, #14448, #10595, #6375, #7040, #11911, #2882, #8870, #1536, #13419, #12676, #1400, #11115, #2480, #4586, #13483, #8867, #10767, #263, #835, #6978, #45, #13703, #7742 ) ) ;
#5191 = CARTESIAN_POINT ( 'NONE',  ( 3.426491571325181340, 1.679378605318042395, -1.679378605318058604 ) ) ;
#5193 = ORIENTED_EDGE ( 'NONE', *, *, #6712, .T. ) ;
#5194 = CARTESIAN_POINT ( 'NONE',  ( 3.426491571325181340, 1.986429008462982093, 0.6339643213050358828 ) ) ;
#5196 = ORIENTED_EDGE ( 'NONE', *, *, #7506, .F. ) ;
#5195 = CARTESIAN_POINT ( 'NONE',  ( 3.602264755523620465, 0.9969999999999996643, -0.4491205543005138412 ) ) ;
#5197 = ORIENTED_EDGE ( 'NONE', *, *, #12405, .T. ) ;
#5198 = CARTESIAN_POINT ( 'NONE',  ( 0.6601485485260571995, -0.07064835164835162051, 0.5137583810202324131 ) ) ;
#5199 =( CONVERSION_BASED_UNIT ( 'INCH', #507 ) LENGTH_UNIT ( ) NAMED_UNIT ( #8539 ) );
#5200 = CARTESIAN_POINT ( 'NONE',  ( 0.6500000000000001332, 0.000000000000000000, 2.968000000000000860 ) ) ;
#5201 = ORIENTED_EDGE ( 'NONE', *, *, #13440, .T. ) ;
#5202 = CARTESIAN_POINT ( 'NONE',  ( 0.09500000000000431710, 1.679378605318059492, 1.679378605318041506 ) ) ;
#5203 = CARTESIAN_POINT ( 'NONE',  ( 3.874999999999999556, 3.137999999999999901, -1.320000000000000062 ) ) ;
#5204 = LINE ( 'NONE', #2984, #6455 ) ;
#5205 = AXIS2_PLACEMENT_3D ( 'NONE', #1930, #9209, #8900 ) ;
#5206 = CARTESIAN_POINT ( 'NONE',  ( 0.7022453151856735687, -0.02852180867591198182, 0.4813241942165198406 ) ) ;
#5207 =( BOUNDED_SURFACE ( )  B_SPLINE_SURFACE ( 3, 2, ( 
 ( #4324, #848, #8910 ),
 ( #769, #622, #11201 ),
 ( #14719, #8995, #5628 ),
 ( #10212, #4469, #6543 ),
 ( #13475, #12421, #5469 ),
 ( #14947, #14871, #9141 ),
 ( #4402, #3017, #6622 ),
 ( #7683, #13554, #9066 ),
 ( #9990, #3243, #11276 ),
 ( #7909, #4247, #12559 ),
 ( #2082, #6770, #13779 ),
 ( #12266, #10341, #4386 ),
 ( #5613, #6676, #12544 ),
 ( #9051, #5683, #12471 ),
 ( #2067, #6757, #14853 ),
 ( #11333, #1989, #11411 ) ),
 .UNSPECIFIED., .F., .F., .F. ) 
 B_SPLINE_SURFACE_WITH_KNOTS ( ( 4, 2, 2, 2, 2, 2, 2, 4 ),
 ( 3, 3 ),
 ( 0.002083263661281769923, 0.002712596804664455137, 0.003341929948047140785, 0.003971263091429826433, 0.004600596234812511648, 0.005229929378195196862, 0.005859262521577882077, 0.007117928808343253373 ),
 ( 0.000000000000000000, 1.000000000000000000 ),
 .UNSPECIFIED. ) 
 GEOMETRIC_REPRESENTATION_ITEM ( )  RATIONAL_B_SPLINE_SURFACE ( (
 ( 1.000000000000000000, 0.8987017906623400165, 1.000000000000000000),
 ( 1.000000000000000000, 0.9020594141850755143, 1.000000000000000000),
 ( 1.000000000000000000, 0.9044651860914172392, 1.000000000000000000),
 ( 1.000000000000000000, 0.9073335834956595125, 1.000000000000000000),
 ( 1.000000000000000000, 0.9077660037303413310, 1.000000000000000000),
 ( 1.000000000000000000, 0.9065807100086308301, 1.000000000000000000),
 ( 1.000000000000000000, 0.9049576633627471889, 1.000000000000000000),
 ( 1.000000000000000000, 0.8998093858009208468, 1.000000000000000000),
 ( 1.000000000000000000, 0.8963317359659079830, 1.000000000000000000),
 ( 1.000000000000000000, 0.8876325024794819996, 1.000000000000000000),
 ( 1.000000000000000000, 0.8824894405370273809, 1.000000000000000000),
 ( 1.000000000000000000, 0.8708860455747078344, 1.000000000000000000),
 ( 1.000000000000000000, 0.8643359190950669069, 1.000000000000000000),
 ( 1.000000000000000000, 0.8432203508677428294, 1.000000000000000000),
 ( 1.000000000000000000, 0.8269334966166562717, 1.000000000000000000),
 ( 1.000000000000000000, 0.8091170061680378334, 1.000000000000000000) ) ) 
 REPRESENTATION_ITEM ( '' )  SURFACE ( )  );
#5208 = EDGE_CURVE ( 'NONE', #6943, #13629, #11346, .T. ) ;
#5209 = DIRECTION ( 'NONE',  ( -0.7071067811865429098, 8.659560562354987092E-17, -0.7071067811865521247 ) ) ;
#5210 = EDGE_CURVE ( 'NONE', #13813, #9131, #10061, .T. ) ;
#5211 = ORIENTED_EDGE ( 'NONE', *, *, #12218, .F. ) ;
#5212 = ADVANCED_FACE ( 'NONE', ( #13637 ), #5207, .F. ) ;
#5213 = DIRECTION ( 'NONE',  ( -0.000000000000000000, -1.000000000000000000, -0.000000000000000000 ) ) ;
#5214 = VERTEX_POINT ( 'NONE', #13694 ) ;
#5215 = CARTESIAN_POINT ( 'NONE',  ( 3.874999999999999556, 3.567999999999999616, 1.320000000000000062 ) ) ;
#5216 = VERTEX_POINT ( 'NONE', #11495 ) ;
#5217 = ADVANCED_FACE ( 'NONE', ( #3229 ), #9817, .F. ) ;
#5218 = EDGE_CURVE ( 'NONE', #1997, #6687, #3464, .T. ) ;
#5219 = CARTESIAN_POINT ( 'NONE',  ( 0.09500000000000431710, 1.679378605318059492, 1.679378605318041506 ) ) ;
#5220 = ORIENTED_EDGE ( 'NONE', *, *, #1360, .F. ) ;
#5221 = CIRCLE ( 'NONE', #69, 2.960629921259842146 ) ;
#5222 = LINE ( 'NONE', #13388, #7570 ) ;
#5223 = VECTOR ( 'NONE', #1312, 39.37007874015748143 ) ;
#5224 = CARTESIAN_POINT ( 'NONE',  ( 0.8039452708728591634, -0.4429999999999999494, -0.3054822237058766876 ) ) ;
#5225 = DIRECTION ( 'NONE',  ( 0.000000000000000000, 1.000000000000000000, -4.591341165821855765E-15 ) ) ;
#5226 = FACE_OUTER_BOUND ( 'NONE', #12784, .T. ) ;
#5227 = CARTESIAN_POINT ( 'NONE',  ( 1.324514161726550343, 5.548674798467436505E-05, -0.4812921728568291257 ) ) ;
#5228 = LENGTH_MEASURE_WITH_UNIT ( LENGTH_MEASURE( 0.02539999999999999897 ), #1770 );
#5229 = AXIS2_PLACEMENT_3D ( 'NONE', #11164, #9951, #6507 ) ;
#5230 = EDGE_LOOP ( 'NONE', ( #825, #570 ) ) ;
#5231 = ORIENTED_EDGE ( 'NONE', *, *, #4401, .T. ) ;
#5232 = VERTEX_POINT ( 'NONE', #10273 ) ;
#5233 = CARTESIAN_POINT ( 'NONE',  ( 8.850000000000001421, 0.8819999999999995621, 6.829619984160658046E-17 ) ) ;
#5234 = ORIENTED_EDGE ( 'NONE', *, *, #11852, .T. ) ;
#5235 = DIRECTION ( 'NONE',  ( 1.000000000000000000, 0.000000000000000000, 0.000000000000000000 ) ) ;
#5236 = EDGE_CURVE ( 'NONE', #14399, #1593, #7893, .T. ) ;
#5237 = DIRECTION ( 'NONE',  ( -1.224646799147353207E-16, 0.000000000000000000, -1.000000000000000000 ) ) ;
#5238 = DIRECTION ( 'NONE',  ( 0.000000000000000000, 0.000000000000000000, 1.000000000000000000 ) ) ;
#5239 = EDGE_CURVE ( 'NONE', #6058, #2380, #4456, .T. ) ;
#5240 = VECTOR ( 'NONE', #7835, 39.37007874015748854 ) ;
#5241 = CARTESIAN_POINT ( 'NONE',  ( 2.980731298636167370, 3.137999999999999901, 0.3249191361593796179 ) ) ;
#5242 = ORIENTED_EDGE ( 'NONE', *, *, #8611, .F. ) ;
#5243 = ORIENTED_EDGE ( 'NONE', *, *, #2043, .T. ) ;
#5244 = AXIS2_PLACEMENT_3D ( 'NONE', #9175, #10173, #2205 ) ;
#5245 = ORIENTED_EDGE ( 'NONE', *, *, #13155, .F. ) ;
#5246 = CARTESIAN_POINT ( 'NONE',  ( 2.124999999999999556, 1.575000000000016165, 2.359999999999999876 ) ) ;
#5247 = VECTOR ( 'NONE', #11036, 39.37007874015748854 ) ;
#5248 = VECTOR ( 'NONE', #5614, 39.37007874015748143 ) ;
#5249 = CYLINDRICAL_SURFACE ( 'NONE', #5549, 0.4349999999999999423 ) ;
#5250 = FACE_OUTER_BOUND ( 'NONE', #3670, .T. ) ;
#5251 = DIRECTION ( 'NONE',  ( 0.000000000000000000, 0.000000000000000000, 1.000000000000000000 ) ) ;
#5252 = EDGE_LOOP ( 'NONE', ( #3776, #3223, #3735, #11103, #7118, #13802, #3624, #5243 ) ) ;
#5253 = FACE_OUTER_BOUND ( 'NONE', #8727, .T. ) ;
#5254 = DIRECTION ( 'NONE',  ( 0.000000000000000000, -1.000000000000000000, 0.000000000000000000 ) ) ;
#5255 = ADVANCED_FACE ( 'NONE', ( #3306 ), #5173, .F. ) ;
#5256 = EDGE_CURVE ( 'NONE', #8543, #1080, #1009, .T. ) ;
#5257 = LINE ( 'NONE', #7554, #4383 ) ;
#5258 = AXIS2_PLACEMENT_3D ( 'NONE', #7374, #1385, #2549 ) ;
#5259 = DIRECTION ( 'NONE',  ( -0.3420201433256627732, 0.000000000000000000, 0.9396926207859105373 ) ) ;
#5260 = AXIS2_PLACEMENT_3D ( 'NONE', #12381, #6364, #8648 ) ;
#5261 = CIRCLE ( 'NONE', #13558, 0.4999999999999997224 ) ;
#5262 = CARTESIAN_POINT ( 'NONE',  ( 0.9658607511226641185, -0.4371914870459378544, -0.4523269952906700531 ) ) ;
#5263 = CARTESIAN_POINT ( 'NONE',  ( 4.426064865072103949, 1.707355206796218328, 0.5795993612514793725 ) ) ;
#5265 = ORIENTED_EDGE ( 'NONE', *, *, #11253, .T. ) ;
#5264 = DIRECTION ( 'NONE',  ( -0.2251194151855826497, -0.9743259920144012876, 0.003179652756858320634 ) ) ;
#5266 = EDGE_LOOP ( 'NONE', ( #6540, #2474, #2550, #11859 ) ) ;
#5267 = CARTESIAN_POINT ( 'NONE',  ( -0.3662050505264201616, 1.600827805288695949, -0.1276197524519294968 ) ) ;
#5269 = ORIENTED_EDGE ( 'NONE', *, *, #10500, .T. ) ;
#5268 = DIRECTION ( 'NONE',  ( -0.000000000000000000, 0.000000000000000000, 1.000000000000000000 ) ) ;
#5270 = EDGE_LOOP ( 'NONE', ( #1851, #4872, #6915, #14680 ) ) ;
#5271 = CARTESIAN_POINT ( 'NONE',  ( 0.6566154142300545393, -0.01187121282287852304, 0.4974659767684405653 ) ) ;
#5272 = AXIS2_PLACEMENT_3D ( 'NONE', #10957, #5076, #6517 ) ;
#5273 = DIRECTION ( 'NONE',  ( 0.000000000000000000, 0.000000000000000000, -1.000000000000000000 ) ) ;
#5274 = ORIENTED_EDGE ( 'NONE', *, *, #2065, .T. ) ;
#5275 = MANIFOLD_SOLID_BREP ( 'CirPattern1', #2284 ) ;
#5276 = CARTESIAN_POINT ( 'NONE',  ( 8.469665986256828205, 0.9969999999999998863, 6.829619984160658046E-17 ) ) ;
#5277 = CARTESIAN_POINT ( 'NONE',  ( 0.6500000000000001332, 1.679378605318035733, -2.086378605318070178 ) ) ;
#5278 = CIRCLE ( 'NONE', #10418, 0.03999999999999994532 ) ;
#5279 = VECTOR ( 'NONE', #7208, 39.37007874015748143 ) ;
#5280 = EDGE_CURVE ( 'NONE', #13770, #13214, #7391, .T. ) ;
#5281 =( REPRESENTATION_RELATIONSHIP ('NONE','NONE', #3591, #1014 ) REPRESENTATION_RELATIONSHIP_WITH_TRANSFORMATION ( #13571 )SHAPE_REPRESENTATION_RELATIONSHIP( ) );
#5282 = FACE_OUTER_BOUND ( 'NONE', #12594, .T. ) ;
#5283 = DIRECTION ( 'NONE',  ( -1.000000000000000000, -0.000000000000000000, -0.000000000000000000 ) ) ;
#5284 = VERTEX_POINT ( 'NONE', #3037 ) ;
#5285 = DIRECTION ( 'NONE',  ( 0.000000000000000000, 0.000000000000000000, -1.000000000000000000 ) ) ;
#5286 = DIRECTION ( 'NONE',  ( -1.000000000000000000, -0.000000000000000000, -0.000000000000000000 ) ) ;
#5287 = EDGE_LOOP ( 'NONE', ( #12352, #9149, #13248, #1966 ) ) ;
#5288 = CARTESIAN_POINT ( 'NONE',  ( 4.126800735551335642, 0.9017823133670000990, -0.4322768681130992330 ) ) ;
#5289 = CARTESIAN_POINT ( 'NONE',  ( -0.2249147617188618498, 1.559103846021574258, 0.3723417112826993836 ) ) ;
#5290 = EDGE_LOOP ( 'NONE', ( #1323, #4297, #7160, #8951 ) ) ;
#5291 = CARTESIAN_POINT ( 'NONE',  ( 5.939536975864662229E-17, 1.239999999999999991, 0.4849999999999999312 ) ) ;
#5292 = ORIENTED_EDGE ( 'NONE', *, *, #12074, .F. ) ;
#5293 = EDGE_CURVE ( 'NONE', #14642, #1037, #2063, .T. ) ;
#5294 = EDGE_CURVE ( 'NONE', #10348, #5886, #10068, .T. ) ;
#5295 = AXIS2_PLACEMENT_3D ( 'NONE', #1588, #11007, #353 ) ;
#5296 = ADVANCED_FACE ( 'NONE', ( #14894 ), #1506, .F. ) ;
#5297 = DIRECTION ( 'NONE',  ( 1.000000000000000000, 0.000000000000000000, 0.000000000000000000 ) ) ;
#5298 = CARTESIAN_POINT ( 'NONE',  ( 1.650520655410188775, 0.1749999999999999889, -0.5816197779170857451 ) ) ;
#5299 = CIRCLE ( 'NONE', #12129, 0.08500000000000004774 ) ;
#5300 = CARTESIAN_POINT ( 'NONE',  ( 3.426491571325181340, 0.000000000000000000, 0.0001794190581142465670 ) ) ;
#5301 = ORIENTED_EDGE ( 'NONE', *, *, #3432, .T. ) ;
#5302 = EDGE_CURVE ( 'NONE', #14113, #8835, #8127, .T. ) ;
#5303 = DIRECTION ( 'NONE',  ( 0.000000000000000000, 1.000000000000000000, -1.836536466328828134E-14 ) ) ;
#5304 = LINE ( 'NONE', #6307, #3247 ) ;
#5305 = DIMENSIONAL_EXPONENTS ( 1.000000000000000000, 0.000000000000000000, 0.000000000000000000, 0.000000000000000000, 0.000000000000000000, 0.000000000000000000, 0.000000000000000000 ) ;
#5306 = CIRCLE ( 'NONE', #13839, 0.1899999999999996136 ) ;
#5307 = FACE_OUTER_BOUND ( 'NONE', #13261, .T. ) ;
#5308 = EDGE_LOOP ( 'NONE', ( #15056, #14065, #4279, #12056, #8441, #8262, #10185, #14923, #6028 ) ) ;
#5309 = EDGE_LOOP ( 'NONE', ( #2270, #4990, #7526, #4068 ) ) ;
#5310 = B_SPLINE_CURVE_WITH_KNOTS ( 'NONE', 3,
 ( #13924, #8138, #4845, #3387, #8066, #9516 ),
 .UNSPECIFIED., .F., .F.,
 ( 4, 2, 4 ),
 ( 0.000000000000000000, 0.0004346861535602710444, 0.0008693723071205420889 ),
 .UNSPECIFIED. ) ;
#5311 = EDGE_LOOP ( 'NONE', ( #11465, #13743, #9308, #9477 ) ) ;
#5312 = VERTEX_POINT ( 'NONE', #2108 ) ;
#5313 = CARTESIAN_POINT ( 'NONE',  ( 3.426491571325181340, 1.679378605318059048, 1.679378605318041506 ) ) ;
#5314 = EDGE_CURVE ( 'NONE', #12204, #694, #1234, .T. ) ;
#5315 = VECTOR ( 'NONE', #5336, 39.37007874015748143 ) ;
#5316 = DIRECTION ( 'NONE',  ( 0.3420201433256621626, 0.000000000000000000, -0.9396926207859108704 ) ) ;
#5317 = PRODUCT_DEFINITION_SHAPE ( 'NONE', 'NONE',  #15159 ) ;
#5318 = CARTESIAN_POINT ( 'NONE',  ( 3.426491571325181784, 2.005325245437683090, -0.6184897574297448797 ) ) ;
#5319 = CARTESIAN_POINT ( 'NONE',  ( 4.369102373712536291, 1.779600098398884445, -0.5677944546462855291 ) ) ;
#5320 = AXIS2_PLACEMENT_3D ( 'NONE', #13539, #14775, #5457 ) ;
#5321 = ORIENTED_EDGE ( 'NONE', *, *, #13841, .F. ) ;
#5322 = AXIS2_PLACEMENT_3D ( 'NONE', #7623, #3118, #8929 ) ;
#5323 = EDGE_CURVE ( 'NONE', #7678, #801, #13497, .T. ) ;
#5324 = ORIENTED_EDGE ( 'NONE', *, *, #5733, .T. ) ;
#5325 = EDGE_LOOP ( 'NONE', ( #4522, #12131, #8476, #1125 ) ) ;
#5326 = EDGE_CURVE ( 'NONE', #13304, #1703, #2191, .T. ) ;
#5327 = EDGE_LOOP ( 'NONE', ( #13816, #14051 ) ) ;
#5328 = CIRCLE ( 'NONE', #8759, 2.500000000000000000 ) ;
#5329 = CARTESIAN_POINT ( 'NONE',  ( 0.2324505233676561755, 1.569549437900746414, -0.3592893892332560402 ) ) ;
#5330 = LINE ( 'NONE', #11990, #5072 ) ;
#5332 = AXIS2_PLACEMENT_3D ( 'NONE', #9587, #6059, #10724 ) ;
#5331 = CARTESIAN_POINT ( 'NONE',  ( 4.180185220126820589, 0.9181503761820097864, 0.3963891770617307686 ) ) ;
#5333 = ITEM_DEFINED_TRANSFORMATION ( 'NONE', 'NONE', #12067,  #8424 ) ;
#5334 = CARTESIAN_POINT ( 'NONE',  ( 2.599715518929141211, 0.7930078835987426356, 0.4632808542523846329 ) ) ;
#5335 = ORIENTED_EDGE ( 'NONE', *, *, #2088, .F. ) ;
#5336 = DIRECTION ( 'NONE',  ( 0.000000000000000000, 4.591341165822166182E-16, 1.000000000000000000 ) ) ;
#5337 = CARTESIAN_POINT ( 'NONE',  ( 0.000000000000000000, 0.04580000000000046534, 0.000000000000000000 ) ) ;
#5338 = DIRECTION ( 'NONE',  ( 1.000000000000000000, 0.000000000000000000, 0.000000000000000000 ) ) ;
#5339 = CARTESIAN_POINT ( 'NONE',  ( 3.426491571325181340, -1.575000000000027489, -2.359999999999989218 ) ) ;
#5340 = AXIS2_PLACEMENT_3D ( 'NONE', #4162, #6679, #13622 ) ;
#5341 = VECTOR ( 'NONE', #12463, 39.37007874015748143 ) ;
#5342 = CIRCLE ( 'NONE', #13638, 0.3750000000000007772 ) ;
#5343 = CARTESIAN_POINT ( 'NONE',  ( 0.6569077226922048762, 0.000000000000000000, -0.4307156577630670280 ) ) ;
#5344 = VECTOR ( 'NONE', #12361, 39.37007874015748143 ) ;
#5345 = DIRECTION ( 'NONE',  ( -1.000000000000000000, -0.000000000000000000, -0.000000000000000000 ) ) ;
#5346 = CARTESIAN_POINT ( 'NONE',  ( 4.215778309529500056, 1.784571035030107167, 0.6698587355277484390 ) ) ;
#5348 = ORIENTED_EDGE ( 'NONE', *, *, #9449, .F. ) ;
#5347 = DIRECTION ( 'NONE',  ( -0.7071067811865429098, 8.659560562354987092E-17, -0.7071067811865521247 ) ) ;
#5349 = EDGE_CURVE ( 'NONE', #3205, #11461, #4193, .T. ) ;
#5350 = EDGE_CURVE ( 'NONE', #8413, #1274, #13195, .T. ) ;
#5351 = ORIENTED_EDGE ( 'NONE', *, *, #1693, .F. ) ;
#5353 = ORIENTED_EDGE ( 'NONE', *, *, #1631, .F. ) ;
#5352 = CARTESIAN_POINT ( 'NONE',  ( 2.230477600021715912, 0.4287871555018993308, -0.4684960790957384824 ) ) ;
#5354 = CIRCLE ( 'NONE', #5118, 0.7849999999999998090 ) ;
#5355 = EDGE_LOOP ( 'NONE', ( #3413, #7771, #8410, #7754 ) ) ;
#5356 = VECTOR ( 'NONE', #13063, 39.37007874015748854 ) ;
#5357 = CARTESIAN_POINT ( 'NONE',  ( -0.09035531712817639061, 1.379999999999999671, -0.1564999999999998892 ) ) ;
#5358 = FACE_OUTER_BOUND ( 'NONE', #653, .T. ) ;
#5359 = ORIENTED_EDGE ( 'NONE', *, *, #4492, .T. ) ;
#5360 = AXIS2_PLACEMENT_3D ( 'NONE', #15039, #786, #1954 ) ;
#5361 = FACE_OUTER_BOUND ( 'NONE', #11272, .T. ) ;
#5362 = LINE ( 'NONE', #580, #6819 ) ;
#5363 = AXIS2_PLACEMENT_3D ( 'NONE', #13255, #14648, #11205 ) ;
#5364 = DIRECTION ( 'NONE',  ( 2.930988785010413267E-14, 0.000000000000000000, -1.000000000000000000 ) ) ;
#5365 = CONICAL_SURFACE ( 'NONE', #9021, 1.000000000000000000, 0.7853981633974517207 ) ;
#5366 = DIRECTION ( 'NONE',  ( 0.000000000000000000, 1.000000000000000000, -8.723548215061523903E-15 ) ) ;
#5367 = DIRECTION ( 'NONE',  ( 1.655665450705613915E-16, 0.000000000000000000, 1.000000000000000000 ) ) ;
#5368 = ORIENTED_EDGE ( 'NONE', *, *, #7219, .F. ) ;
#5369 = DIRECTION ( 'NONE',  ( 0.000000000000000000, 0.000000000000000000, -1.000000000000000000 ) ) ;
#5370 = AXIS2_PLACEMENT_3D ( 'NONE', #4607, #15001, #3301 ) ;
#5371 = DIRECTION ( 'NONE',  ( -1.000000000000000000, -0.000000000000000000, -0.000000000000000000 ) ) ;
#5372 = DIRECTION ( 'NONE',  ( 1.000000000000000000, 0.000000000000000000, 0.000000000000000000 ) ) ;
#5373 = CARTESIAN_POINT ( 'NONE',  ( 0.6179999999999965521, -1.679378605318047946, -2.054378605318054163 ) ) ;
#5374 = EDGE_LOOP ( 'NONE', ( #2846, #2660, #11600, #7880, #14609 ) ) ;
#5375 = EDGE_CURVE ( 'NONE', #3743, #2839, #6626, .T. ) ;
#5376 = CARTESIAN_POINT ( 'NONE',  ( 3.875000000000000000, 0.8660254037844385966, -0.5000000000000002220 ) ) ;
#5377 = CARTESIAN_POINT ( 'NONE',  ( 2.774999999999999911, 1.575000000000000178, -2.360000000000016751 ) ) ;
#5378 = ORIENTED_EDGE ( 'NONE', *, *, #5350, .F. ) ;
#5379 = CYLINDRICAL_SURFACE ( 'NONE', #794, 0.1899999999999996136 ) ;
#5380 = LINE ( 'NONE', #6603, #4388 ) ;
#5381 = DIRECTION ( 'NONE',  ( 2.602462600580852055E-17, 1.000000000000000000, -4.814436796019480615E-35 ) ) ;
#5382 = AXIS2_PLACEMENT_3D ( 'NONE', #2929, #11031, #13236 ) ;
#5383 = DIRECTION ( 'NONE',  ( 0.000000000000000000, 0.000000000000000000, 1.000000000000000000 ) ) ;
#5384 = DIRECTION ( 'NONE',  ( 0.000000000000000000, 0.000000000000000000, -1.000000000000000000 ) ) ;
#5385 = CARTESIAN_POINT ( 'NONE',  ( 0.9659751558686909823, -0.4829425875655894429, -0.4106976866094356193 ) ) ;
#5386 = ORIENTED_EDGE ( 'NONE', *, *, #3906, .F. ) ;
#5387 = DIRECTION ( 'NONE',  ( -1.000000000000000000, -0.000000000000000000, -0.000000000000000000 ) ) ;
#5388 = DIRECTION ( 'NONE',  ( 0.000000000000000000, 0.000000000000000000, 1.000000000000000000 ) ) ;
#5389 =( NAMED_UNIT ( * ) SI_UNIT ( $, .STERADIAN. ) SOLID_ANGLE_UNIT ( ) );
#5390 = CARTESIAN_POINT ( 'NONE',  ( 3.426491571325181340, -1.575000000000027489, -1.574999999999989297 ) ) ;
#5391 = ORIENTED_EDGE ( 'NONE', *, *, #11125, .F. ) ;
#5392 = ORIENTED_EDGE ( 'NONE', *, *, #4420, .T. ) ;
#5393 = DIRECTION ( 'NONE',  ( -0.000000000000000000, -1.000000000000000000, 0.000000000000000000 ) ) ;
#5394 = VERTEX_POINT ( 'NONE', #7179 ) ;
#5395 = CARTESIAN_POINT ( 'NONE',  ( 1.375000000000000000, 0.000000000000000000, 1.350000000000000089 ) ) ;
#5396 = DIRECTION ( 'NONE',  ( -1.000000000000000000, -0.000000000000000000, -0.000000000000000000 ) ) ;
#5397 = CARTESIAN_POINT ( 'NONE',  ( 0.1250000000000009992, 0.000000000000000000, 0.000000000000000000 ) ) ;
#5398 = CARTESIAN_POINT ( 'NONE',  ( 4.548534283101781206, 1.796214626747565601, 0.3340040616788196304 ) ) ;
#5399 = ORIENTED_EDGE ( 'NONE', *, *, #14306, .T. ) ;
#5400 = ADVANCED_FACE ( 'NONE', ( #12815 ), #9396, .F. ) ;
#5401 = EDGE_CURVE ( 'NONE', #8878, #13854, #10535, .T. ) ;
#5402 = EDGE_CURVE ( 'NONE', #1776, #9581, #10457, .T. ) ;
#5403 = ORIENTED_EDGE ( 'NONE', *, *, #9625, .T. ) ;
#5404 = ORIENTED_EDGE ( 'NONE', *, *, #52, .F. ) ;
#5405 = UNCERTAINTY_MEASURE_WITH_UNIT (LENGTH_MEASURE( 1.000000000000000082E-05 ), #6729, 'distance_accuracy_value', 'NONE');
#5406 = ORIENTED_EDGE ( 'NONE', *, *, #7859, .F. ) ;
#5407 = AXIS2_PLACEMENT_3D ( 'NONE', #13785, #14951, #7997 ) ;
#5408 = CARTESIAN_POINT ( 'NONE',  ( 3.875000000000000000, 3.137999999999999901, 0.000000000000000000 ) ) ;
#5409 = DIRECTION ( 'NONE',  ( -0.9992912762382413216, -0.03489602031262312859, -0.01411428356268701854 ) ) ;
#5410 = CARTESIAN_POINT ( 'NONE',  ( 2.124999999999999556, 3.360000000000016751, 0.9799999999999461364 ) ) ;
#5411 = EDGE_CURVE ( 'NONE', #10222, #2606, #12967, .T. ) ;
#5412 = CONTEXT_DEPENDENT_SHAPE_REPRESENTATION ( #7621, #13477 ) ;
#5413 = CARTESIAN_POINT ( 'NONE',  ( 3.906623289280057325E-17, 1.159999999999999698, 0.3190000000000000058 ) ) ;
#5414 = ORIENTED_EDGE ( 'NONE', *, *, #5066, .T. ) ;
#5415 = LINE ( 'NONE', #13574, #12893 ) ;
#5416 = DIRECTION ( 'NONE',  ( 0.000000000000000000, 0.000000000000000000, -1.000000000000000000 ) ) ;
#5417 = DIRECTION ( 'NONE',  ( 0.4961857140186716753, 0.000000000000000000, -0.8682164115033653706 ) ) ;
#5418 = CARTESIAN_POINT ( 'NONE',  ( 0.7067472695984848841, -0.05999999999999994227, -0.5500236785040136800 ) ) ;
#5419 = AXIS2_PLACEMENT_3D ( 'NONE', #4642, #15038, #9311 ) ;
#5420 = CARTESIAN_POINT ( 'NONE',  ( 8.802840746862891308, 0.9385542876807514423, 0.1899546695978080457 ) ) ;
#5421 = CARTESIAN_POINT ( 'NONE',  ( 0.9999999999999993339, -0.4429999999999999494, 0.4258697216429003785 ) ) ;
#5422 = CARTESIAN_POINT ( 'NONE',  ( 1.000048944713735732, -0.4428998280398805387, -0.4293350073753851581 ) ) ;
#5423 = CARTESIAN_POINT ( 'NONE',  ( 4.316286828030351685, 1.708216954940201759, 0.6629077590058020109 ) ) ;
#5425 = VERTEX_POINT ( 'NONE', #14037 ) ;
#5424 = CARTESIAN_POINT ( 'NONE',  ( 3.874999999999999556, 3.535499999999999421, 1.320000000000000062 ) ) ;
#5426 = ORIENTED_EDGE ( 'NONE', *, *, #15086, .F. ) ;
#5428 = VERTEX_POINT ( 'NONE', #4572 ) ;
#5427 = DIRECTION ( 'NONE',  ( 0.000000000000000000, 0.000000000000000000, -1.000000000000000000 ) ) ;
#5429 = ORIENTED_EDGE ( 'NONE', *, *, #12903, .T. ) ;
#5430 = EDGE_CURVE ( 'NONE', #12094, #5284, #3443, .T. ) ;
#5431 = DIRECTION ( 'NONE',  ( 0.000000000000000000, 0.000000000000000000, -1.000000000000000000 ) ) ;
#5432 = PLANE ( 'NONE',  #5022 ) ;
#5433 = ORIENTED_EDGE ( 'NONE', *, *, #1360, .T. ) ;
#5434 = DIRECTION ( 'NONE',  ( 0.000000000000000000, 1.000000000000000000, -0.000000000000000000 ) ) ;
#5435 = CARTESIAN_POINT ( 'NONE',  ( 0.6179999999999965521, 1.679378605318059492, 2.054378605318042172 ) ) ;
#5436 = EDGE_CURVE ( 'NONE', #5706, #1342, #12714, .T. ) ;
#5437 = EDGE_CURVE ( 'NONE', #2400, #1562, #1031, .T. ) ;
#5438 = CARTESIAN_POINT ( 'NONE',  ( 3.470516203624053997, 1.056999999999999718, -0.3909199583802889233 ) ) ;
#5439 = CARTESIAN_POINT ( 'NONE',  ( 0.9682282713927263806, -0.4430792971874000230, -0.3432655056157467022 ) ) ;
#5440 = CIRCLE ( 'NONE', #5932, 0.1900000000000000577 ) ;
#5441 = VERTEX_POINT ( 'NONE', #12739 ) ;
#5442 = DIRECTION ( 'NONE',  ( 0.000000000000000000, 0.000000000000000000, -1.000000000000000000 ) ) ;
#5443 = CARTESIAN_POINT ( 'NONE',  ( 3.696710981162860676, 0.8840651821477499839, -0.4674177165474920903 ) ) ;
#5444 = CARTESIAN_POINT ( 'NONE',  ( 4.449168964073242805, 1.708272156618657833, -0.5570130099483981967 ) ) ;
#5445 = ORIENTED_EDGE ( 'NONE', *, *, #1959, .T. ) ;
#5446 = DIRECTION ( 'NONE',  ( 0.000000000000000000, -1.000000000000000000, 0.000000000000000000 ) ) ;
#5447 = DIRECTION ( 'NONE',  ( 1.000000000000000000, 0.000000000000000000, 0.000000000000000000 ) ) ;
#5448 = CIRCLE ( 'NONE', #13976, 0.3440000000000000280 ) ;
#5449 = VERTEX_POINT ( 'NONE', #1188 ) ;
#5450 = CIRCLE ( 'NONE', #3979, 0.5000000000000000000 ) ;
#5451 = CARTESIAN_POINT ( 'NONE',  ( 6.826491571325181695, 1.679378605318035733, -1.679378605318065487 ) ) ;
#5452 = VERTEX_POINT ( 'NONE', #9550 ) ;
#5453 = DIRECTION ( 'NONE',  ( 0.000000000000000000, 0.000000000000000000, -1.000000000000000000 ) ) ;
#5454 = VECTOR ( 'NONE', #6383, 39.37007874015748854 ) ;
#5455 = LINE ( 'NONE', #2209, #4403 ) ;
#5456 = EDGE_CURVE ( 'NONE', #8139, #3117, #13958, .T. ) ;
#5457 = DIRECTION ( 'NONE',  ( 0.000000000000000000, 0.000000000000000000, 1.000000000000000000 ) ) ;
#5458 = CARTESIAN_POINT ( 'NONE',  ( 0.9662251482428009242, -0.4440312122665853733, -0.4102559963803746323 ) ) ;
#5459 = ORIENTED_EDGE ( 'NONE', *, *, #14409, .F. ) ;
#5460 = CARTESIAN_POINT ( 'NONE',  ( 0.6500000000000001332, -1.679378605318047946, -2.086378605318057744 ) ) ;
#5461 = DIRECTION ( 'NONE',  ( 1.655665450705613915E-16, 3.103226861728128995E-32, 1.000000000000000000 ) ) ;
#5462 = CYLINDRICAL_SURFACE ( 'NONE', #12342, 2.500000000000000444 ) ;
#5463 = ORIENTED_EDGE ( 'NONE', *, *, #13258, .F. ) ;
#5464 = ORIENTED_EDGE ( 'NONE', *, *, #4785, .F. ) ;
#5465 = CARTESIAN_POINT ( 'NONE',  ( 1.000081574522892591, -0.4828330467331338194, -0.4316451978637083631 ) ) ;
#5466 = EDGE_LOOP ( 'NONE', ( #1236, #5989, #8230, #699 ) ) ;
#5467 = FACE_OUTER_BOUND ( 'NONE', #6584, .T. ) ;
#5468 = AXIS2_PLACEMENT_3D ( 'NONE', #14173, #10664, #10 ) ;
#5469 = CARTESIAN_POINT ( 'NONE',  ( 0.7007173259568594270, -0.4032680294360234674, -0.4867265490097360536 ) ) ;
#5470 = CIRCLE ( 'NONE', #8647, 0.9499999999999992895 ) ;
#5471 = DIRECTION ( 'NONE',  ( 0.000000000000000000, 0.000000000000000000, 1.000000000000000000 ) ) ;
#5472 = CARTESIAN_POINT ( 'NONE',  ( 2.774999999999999911, 0.000000000000000000, 2.500000000000000444 ) ) ;
#5473 = EDGE_CURVE ( 'NONE', #9898, #15127, #10608, .T. ) ;
#5474 = EDGE_LOOP ( 'NONE', ( #8915, #7564, #6800, #6958 ) ) ;
#5475 = CIRCLE ( 'NONE', #10592, 0.1250000000000000278 ) ;
#5476 = AXIS2_PLACEMENT_3D ( 'NONE', #5810, #14980, #1272 ) ;
#5477 = ORIENTED_EDGE ( 'NONE', *, *, #3166, .F. ) ;
#5478 = ORIENTED_EDGE ( 'NONE', *, *, #9536, .T. ) ;
#5479 = VERTEX_POINT ( 'NONE', #4801 ) ;
#5480 = DIRECTION ( 'NONE',  ( -0.4999999999999979461, 0.000000000000000000, 0.8660254037844397068 ) ) ;
#5481 = DIRECTION ( 'NONE',  ( -1.000000000000000000, -0.000000000000000000, -0.000000000000000000 ) ) ;
#5482 = CARTESIAN_POINT ( 'NONE',  ( -0.4424999999999983946, -0.6590000000000000302, -0.3725000000000000533 ) ) ;
#5483 = CARTESIAN_POINT ( 'NONE',  ( -0.03634916050344735167, 1.602949386431022694, 0.3809527529760086684 ) ) ;
#5484 = ORIENTED_EDGE ( 'NONE', *, *, #4145, .T. ) ;
#5485 = VECTOR ( 'NONE', #8498, 39.37007874015748143 ) ;
#5486 = CARTESIAN_POINT ( 'NONE',  ( 2.124999999999999556, 1.679378605318042395, -1.973878605318058588 ) ) ;
#5487 = EDGE_CURVE ( 'NONE', #3922, #9279, #3744, .T. ) ;
#5488 = ADVANCED_FACE ( 'NONE', ( #2264 ), #479, .T. ) ;
#5489 = DIRECTION ( 'NONE',  ( 1.000000000000000000, 0.000000000000000000, 0.000000000000000000 ) ) ;
#5490 = EDGE_CURVE ( 'NONE', #7156, #7967, #6382, .T. ) ;
#5491 = PRESENTATION_STYLE_ASSIGNMENT (( #7858 ) ) ;
#5492 = FACE_OUTER_BOUND ( 'NONE', #10284, .T. ) ;
#5493 = ADVANCED_FACE ( 'NONE', ( #4650 ), #7254, .F. ) ;
#5494 = AXIS2_PLACEMENT_3D ( 'NONE', #5137, #13290, #12379 ) ;
#5495 = CARTESIAN_POINT ( 'NONE',  ( 4.350709184091345882, 1.779665969747238785, 0.5813850623748166857 ) ) ;
#5496 = AXIS2_PLACEMENT_3D ( 'NONE', #4460, #11337, #9127 ) ;
#5498 = EDGE_LOOP ( 'NONE', ( #3320, #4900, #5477, #10312 ) ) ;
#5497 = FACE_BOUND ( 'NONE', #818, .T. ) ;
#5499 = CIRCLE ( 'NONE', #13546, 0.4849999999999995981 ) ;
#5500 = ORIENTED_EDGE ( 'NONE', *, *, #10850, .T. ) ;
#5502 = ORIENTED_EDGE ( 'NONE', *, *, #7760, .T. ) ;
#5501 = FACE_OUTER_BOUND ( 'NONE', #6798, .T. ) ;
#5503 = ORIENTED_EDGE ( 'NONE', *, *, #6712, .F. ) ;
#5504 = DIRECTION ( 'NONE',  ( -0.7071067811865479058, 0.000000000000000000, 0.7071067811865471286 ) ) ;
#5505 = DIRECTION ( 'NONE',  ( 0.000000000000000000, 0.000000000000000000, 1.000000000000000000 ) ) ;
#5506 = VERTEX_POINT ( 'NONE', #14117 ) ;
#5507 = DIRECTION ( 'NONE',  ( 0.7071067811865429098, 8.659560562354987092E-17, 0.7071067811865521247 ) ) ;
#5508 = PLANE ( 'NONE',  #11455 ) ;
#5509 = AXIS2_PLACEMENT_3D ( 'NONE', #12682, #5735, #12599 ) ;
#5510 = AXIS2_PLACEMENT_3D ( 'NONE', #15096, #6002, #10516 ) ;
#5511 = CIRCLE ( 'NONE', #11362, 2.500000000000000000 ) ;
#5512 = CARTESIAN_POINT ( 'NONE',  ( 2.980731298636167370, 3.137999999999999901, 0.3249191361593797844 ) ) ;
#5513 = DIRECTION ( 'NONE',  ( 0.000000000000000000, 0.000000000000000000, -1.000000000000000000 ) ) ;
#5514 = EDGE_LOOP ( 'NONE', ( #11533, #10066 ) ) ;
#5515 = CARTESIAN_POINT ( 'NONE',  ( -0.2100000000000001865, 1.239999999999999991, 0.3809527529760087239 ) ) ;
#5516 = CARTESIAN_POINT ( 'NONE',  ( 3.436969365618575800, 1.985569024027678875, 0.2422625011488116487 ) ) ;
#5517 = DIRECTION ( 'NONE',  ( 0.7071067811865460184, 0.000000000000000000, -0.7071067811865490160 ) ) ;
#5518 = EDGE_CURVE ( 'NONE', #2976, #6934, #3198, .T. ) ;
#5519 = CIRCLE ( 'NONE', #10158, 1.000000000000000000 ) ;
#5520 = DIRECTION ( 'NONE',  ( -1.000000000000000000, -0.000000000000000000, -0.000000000000000000 ) ) ;
#5521 = DIRECTION ( 'NONE',  ( 0.000000000000000000, -1.000000000000000000, 1.423315761404775650E-14 ) ) ;
#5522 = ORIENTED_EDGE ( 'NONE', *, *, #13879, .T. ) ;
#5523 = CIRCLE ( 'NONE', #13564, 0.1899999999999999745 ) ;
#5524 = VECTOR ( 'NONE', #14415, 39.37007874015748854 ) ;
#5525 = EDGE_CURVE ( 'NONE', #13304, #4332, #8338, .T. ) ;
#5526 = CARTESIAN_POINT ( 'NONE',  ( 7.144847001653046861E-17, -0.6334543218446814228, 0.000000000000000000 ) ) ;
#5527 = ORIENTED_EDGE ( 'NONE', *, *, #2964, .T. ) ;
#5528 = DIRECTION ( 'NONE',  ( 0.000000000000000000, -1.000000000000000000, 0.000000000000000000 ) ) ;
#5529 = AXIS2_PLACEMENT_3D ( 'NONE', #14845, #13610, #7886 ) ;
#5530 = CARTESIAN_POINT ( 'NONE',  ( 0.000000000000000000, 0.000000000000000000, 0.000000000000000000 ) ) ;
#5531 = CARTESIAN_POINT ( 'NONE',  ( 3.426491571325181340, 0.9799999999999438050, -2.360000000000016307 ) ) ;
#5532 = FACE_OUTER_BOUND ( 'NONE', #11959, .T. ) ;
#5533 = AXIS2_PLACEMENT_3D ( 'NONE', #10441, #87, #6007 ) ;
#5534 = CIRCLE ( 'NONE', #2843, 2.968000000000000860 ) ;
#5535 = ORIENTED_EDGE ( 'NONE', *, *, #1083, .T. ) ;
#5536 = DIRECTION ( 'NONE',  ( 0.000000000000000000, 0.000000000000000000, 1.000000000000000000 ) ) ;
#5537 = DIRECTION ( 'NONE',  ( -1.000000000000000000, -0.000000000000000000, -0.000000000000000000 ) ) ;
#5538 = CARTESIAN_POINT ( 'NONE',  ( 2.774999999999999911, -0.9799999999999436939, 2.360000000000016307 ) ) ;
#5539 = ORIENTED_EDGE ( 'NONE', *, *, #10356, .F. ) ;
#5540 = ORIENTED_EDGE ( 'NONE', *, *, #10810, .F. ) ;
#5541 = CARTESIAN_POINT ( 'NONE',  ( 0.3724999999999999423, -0.6290000000000003366, 0.4124999999999999223 ) ) ;
#5542 = ADVANCED_FACE ( 'NONE', ( #1334 ), #14672, .F. ) ;
#5543 = ADVANCED_FACE ( 'NONE', ( #10123 ), #5900, .F. ) ;
#5544 = VECTOR ( 'NONE', #5806, 39.37007874015748143 ) ;
#5545 = CARTESIAN_POINT ( 'NONE',  ( 3.426491571325181340, 2.197249752256450025E-20, -0.0001794190581142465670 ) ) ;
#5546 = VERTEX_POINT ( 'NONE', #3164 ) ;
#5547 = PLANE ( 'NONE',  #826 ) ;
#5548 = FACE_OUTER_BOUND ( 'NONE', #2896, .T. ) ;
#5549 = AXIS2_PLACEMENT_3D ( 'NONE', #13421, #2955, #7617 ) ;
#5550 = LINE ( 'NONE', #7762, #13649 ) ;
#5551 = CARTESIAN_POINT ( 'NONE',  ( 4.066623985734413971, 1.805393779619291594, -0.7271255666244380578 ) ) ;
#5552 = ORIENTED_EDGE ( 'NONE', *, *, #7455, .T. ) ;
#5553 = MANIFOLD_SOLID_BREP ( 'Chamfer1', #11825 ) ;
#5554 = ORIENTED_EDGE ( 'NONE', *, *, #14653, .F. ) ;
#5555 = ORIENTED_EDGE ( 'NONE', *, *, #680, .T. ) ;
#5556 = UNCERTAINTY_MEASURE_WITH_UNIT (LENGTH_MEASURE( 1.000000000000000082E-05 ), #1489, 'distance_accuracy_value', 'NONE');
#5557 = CARTESIAN_POINT ( 'NONE',  ( 3.601417382415921686, 1.057000000000000162, 0.5000000000000000000 ) ) ;
#5558 = VERTEX_POINT ( 'NONE', #4307 ) ;
#5559 = DIRECTION ( 'NONE',  ( 0.000000000000000000, 0.000000000000000000, 1.000000000000000000 ) ) ;
#5560 = DIRECTION ( 'NONE',  ( 0.000000000000000000, 0.000000000000000000, -1.000000000000000000 ) ) ;
#5561 = DIRECTION ( 'NONE',  ( -0.000000000000000000, -1.000000000000000000, -0.000000000000000000 ) ) ;
#5562 = CARTESIAN_POINT ( 'NONE',  ( 0.1950126918253253516, 1.569501570604563856, -0.3809527529760087239 ) ) ;
#5563 = ORIENTED_EDGE ( 'NONE', *, *, #6303, .F. ) ;
#5564 = CARTESIAN_POINT ( 'NONE',  ( 3.219323625916810538, 2.473723010511407860, 0.3624492852859261816 ) ) ;
#5565 = DIRECTION ( 'NONE',  ( 0.000000000000000000, 0.000000000000000000, -1.000000000000000000 ) ) ;
#5566 =( NAMED_UNIT ( * ) SI_UNIT ( $, .STERADIAN. ) SOLID_ANGLE_UNIT ( ) );
#5567 = AXIS2_PLACEMENT_3D ( 'NONE', #11140, #12065, #3034 ) ;
#5568 = CYLINDRICAL_SURFACE ( 'NONE', #7850, 0.4849999999999995981 ) ;
#5569 = DIRECTION ( 'NONE',  ( -0.000000000000000000, -1.000000000000000000, -0.000000000000000000 ) ) ;
#5570 = CARTESIAN_POINT ( 'NONE',  ( 4.048339038639393372, 1.809465041664403362, 0.7309204628693353190 ) ) ;
#5571 = ADVANCED_FACE ( 'NONE', ( #8978 ), #254, .T. ) ;
#5573 = VERTEX_POINT ( 'NONE', #2728 ) ;
#5572 = CARTESIAN_POINT ( 'NONE',  ( 3.651698974834499012, 1.959955860919708748, -0.4475141391230971766 ) ) ;
#5574 = CONICAL_SURFACE ( 'NONE', #9237, 0.3750000000000004996, 0.7853981633974621568 ) ;
#5575 = ORIENTED_EDGE ( 'NONE', *, *, #11976, .F. ) ;
#5577 = EDGE_LOOP ( 'NONE', ( #3147, #5736, #11409, #10126 ) ) ;
#5576 = CARTESIAN_POINT ( 'NONE',  ( 2.633526947634466708, 0.3620998228882749692, -0.4033965501631930906 ) ) ;
#5578 = ORIENTED_EDGE ( 'NONE', *, *, #9575, .F. ) ;
#5579 = VECTOR ( 'NONE', #7287, 39.37007874015748143 ) ;
#5580 = CARTESIAN_POINT ( 'NONE',  ( -0.09035531712817639061, 1.629999999999999893, -0.1564999999999998892 ) ) ;
#5581 =( LENGTH_UNIT ( ) NAMED_UNIT ( * ) SI_UNIT ( $, .METRE. ) );
#5582 = CARTESIAN_POINT ( 'NONE',  ( 2.124999999999999556, -1.575000000000027489, -1.574999999999989297 ) ) ;
#5583 = ORIENTED_EDGE ( 'NONE', *, *, #14850, .F. ) ;
#5584 = MANIFOLD_SOLID_BREP ( 'Fillet3', #2781 ) ;
#5585 = LINE ( 'NONE', #6656, #1580 ) ;
#5586 = CARTESIAN_POINT ( 'NONE',  ( 2.774999999999999911, 0.000000000000000000, 2.500000000000000444 ) ) ;
#5587 = CIRCLE ( 'NONE', #6568, 0.5000000000000000000 ) ;
#5588 = ADVANCED_FACE ( 'NONE', ( #6526 ), #4234, .F. ) ;
#5589 = AXIS2_PLACEMENT_3D ( 'NONE', #7929, #12576, #3335 ) ;
#5590 = LINE ( 'NONE', #15064, #309 ) ;
#5591 = DIRECTION ( 'NONE',  ( 0.000000000000000000, 0.000000000000000000, 1.000000000000000000 ) ) ;
#5592 = CARTESIAN_POINT ( 'NONE',  ( 2.230477600021715023, 0.4287871555018993308, -0.4684960790957384824 ) ) ;
#5593 = ORIENTED_EDGE ( 'NONE', *, *, #6965, .T. ) ;
#5594 = DIRECTION ( 'NONE',  ( 0.000000000000000000, 0.000000000000000000, -1.000000000000000000 ) ) ;
#5595 = AXIS2_PLACEMENT_3D ( 'NONE', #13007, #6291, #4994 ) ;
#5596 = DIRECTION ( 'NONE',  ( 0.03489949670248613384, -0.9993908270190963172, 0.000000000000000000 ) ) ;
#5597 = ADVANCED_FACE ( 'NONE', ( #13538 ), #4929, .F. ) ;
#5598 = CIRCLE ( 'NONE', #14628, 0.03999999999999998002 ) ;
#5599 = CARTESIAN_POINT ( 'NONE',  ( 3.784081183264448978, 1.807375528223629235, -0.7960544091624519591 ) ) ;
#5600 = EDGE_CURVE ( 'NONE', #5506, #1362, #13448, .T. ) ;
#5601 = CIRCLE ( 'NONE', #9518, 0.2625000000000000111 ) ;
#5602 = CARTESIAN_POINT ( 'NONE',  ( 0.6179999999999965521, -1.679378605318047946, -1.679378605318053497 ) ) ;
#5604 = ORIENTED_EDGE ( 'NONE', *, *, #13901, .F. ) ;
#5603 = FACE_OUTER_BOUND ( 'NONE', #4755, .T. ) ;
#5605 = ORIENTED_EDGE ( 'NONE', *, *, #10635, .F. ) ;
#5606 = VECTOR ( 'NONE', #4902, 39.37007874015748143 ) ;
#5607 = CARTESIAN_POINT ( 'NONE',  ( 3.426491571325181340, 0.000000000000000000, 2.000179419058113695 ) ) ;
#5608 = AXIS2_PLACEMENT_3D ( 'NONE', #5793, #9318, #8172 ) ;
#5609 = CARTESIAN_POINT ( 'NONE',  ( 6.794491571325179891, 1.679378605318035733, -1.679378605318065487 ) ) ;
#5610 = EDGE_CURVE ( 'NONE', #11384, #15151, #14438, .T. ) ;
#5611 = CARTESIAN_POINT ( 'NONE',  ( 6.826491571325181695, 0.000000000000000000, -1.039370078740158965 ) ) ;
#5612 = ADVANCED_FACE ( 'NONE', ( #11148 ), #875, .F. ) ;
#5613 = CARTESIAN_POINT ( 'NONE',  ( 0.6766938413712969558, -0.4746063864208611704, -0.4478646436804322173 ) ) ;
#5614 = DIRECTION ( 'NONE',  ( -0.7071067811865342501, -0.7071067811865607844, 0.000000000000000000 ) ) ;
#5615 = VECTOR ( 'NONE', #2228, 39.37007874015748143 ) ;
#5616 = MANIFOLD_SOLID_BREP ( 'Cut-Revolve1', #10599 ) ;
#5617 = CIRCLE ( 'NONE', #6346, 0.2624999999999997335 ) ;
#5618 = ORIENTED_EDGE ( 'NONE', *, *, #9134, .T. ) ;
#5619 = DIRECTION ( 'NONE',  ( 0.000000000000000000, 0.000000000000000000, -1.000000000000000000 ) ) ;
#5620 = DIRECTION ( 'NONE',  ( -0.000000000000000000, -1.000000000000000000, -0.000000000000000000 ) ) ;
#5621 = CARTESIAN_POINT ( 'NONE',  ( 2.743000000000000327, 1.679378605318042395, -1.416878605318059314 ) ) ;
#5622 = ORIENTED_EDGE ( 'NONE', *, *, #468, .F. ) ;
#5623 = DIRECTION ( 'NONE',  ( 0.000000000000000000, 0.000000000000000000, 1.000000000000000000 ) ) ;
#5624 = DIRECTION ( 'NONE',  ( 1.000000000000000000, 0.000000000000000000, 3.491481338843133355E-15 ) ) ;
#5625 = ORIENTED_EDGE ( 'NONE', *, *, #9407, .T. ) ;
#5626 = DIRECTION ( 'NONE',  ( -0.9659258262890699775, 3.169619151431688520E-17, -0.2588190451025145222 ) ) ;
#5627 = EDGE_CURVE ( 'NONE', #6554, #12746, #1477, .T. ) ;
#5628 = CARTESIAN_POINT ( 'NONE',  ( 0.7026404547606078799, -0.3911504053871472375, -0.4896627279036659397 ) ) ;
#5629 = CIRCLE ( 'NONE', #10505, 0.4070000000000000839 ) ;
#5630 = CARTESIAN_POINT ( 'NONE',  ( 0.8896579858124370466, -0.4298343112707130875, -0.4649362184193211456 ) ) ;
#5631 = ADVANCED_FACE ( 'NONE', ( #10973 ), #4938, .F. ) ;
#5632 = CARTESIAN_POINT ( 'NONE',  ( 6.826491571325181695, -1.679378605318047946, -2.054378605318054163 ) ) ;
#5633 = ADVANCED_FACE ( 'NONE', ( #4928 ), #153, .F. ) ;
#5634 = VERTEX_POINT ( 'NONE', #3542 ) ;
#5635 = CARTESIAN_POINT ( 'NONE',  ( 3.758446757606395572, 1.898527427273793533, -0.7408372069486923728 ) ) ;
#5636 = ORIENTED_EDGE ( 'NONE', *, *, #11972, .T. ) ;
#5637 = VERTEX_POINT ( 'NONE', #7079 ) ;
#5638 = DIRECTION ( 'NONE',  ( -1.000000000000000000, -0.000000000000000000, -0.000000000000000000 ) ) ;
#5639 = ORIENTED_EDGE ( 'NONE', *, *, #12511, .T. ) ;
#5640 = CARTESIAN_POINT ( 'NONE',  ( 0.8999999999999999112, -0.6429999999999999050, -0.3750000000000000555 ) ) ;
#5641 = CARTESIAN_POINT ( 'NONE',  ( 3.875000000000000000, 3.085321731235734610, 0.4849999999999995981 ) ) ;
#5642 = CARTESIAN_POINT ( 'NONE',  ( 0.8999999999999998002, 0.1749999999999999889, -0.3799999999999999489 ) ) ;
#5643 = CARTESIAN_POINT ( 'NONE',  ( -0.4108223460329260557, 0.000000000000000000, -0.2850000000000041944 ) ) ;
#5644 = ORIENTED_EDGE ( 'NONE', *, *, #14592, .F. ) ;
#5645 = CARTESIAN_POINT ( 'NONE',  ( 3.874999999999999556, 3.137999999999999901, -1.320000000000000062 ) ) ;
#5646 = B_SPLINE_CURVE_WITH_KNOTS ( 'NONE', 3,
 ( #13919, #14157, #1293, #5980 ),
 .UNSPECIFIED., .F., .F.,
 ( 4, 4 ),
 ( 2.044667804973039983E-07, 0.001808351910784379481 ),
 .UNSPECIFIED. ) ;
#5647 = CARTESIAN_POINT ( 'NONE',  ( 0.7007157546338746990, -0.03969898687429768841, -0.4867155808989070409 ) ) ;
#5648 = CARTESIAN_POINT ( 'NONE',  ( 8.661818191809109280, 0.8754285464536269989, -0.3176815264168135200 ) ) ;
#5649 = EDGE_CURVE ( 'NONE', #10545, #14846, #256, .T. ) ;
#5650 = DIRECTION ( 'NONE',  ( -0.9999002670844989726, 0.000000000000000000, -0.01412288512831212997 ) ) ;
#5651 = AXIS2_PLACEMENT_3D ( 'NONE', #2678, #1583, #423 ) ;
#5653 = VERTEX_POINT ( 'NONE', #2475 ) ;
#5652 = FACE_OUTER_BOUND ( 'NONE', #11885, .T. ) ;
#5654 = ORIENTED_EDGE ( 'NONE', *, *, #5767, .T. ) ;
#5656 = ORIENTED_EDGE ( 'NONE', *, *, #2507, .T. ) ;
#5655 = CARTESIAN_POINT ( 'NONE',  ( 3.874999999999999556, 2.750000000000000000, -1.820000000000000284 ) ) ;
#5657 = ORIENTED_EDGE ( 'NONE', *, *, #3528, .F. ) ;
#5658 = DIRECTION ( 'NONE',  ( 0.000000000000000000, 0.000000000000000000, -1.000000000000000000 ) ) ;
#5659 = DIRECTION ( 'NONE',  ( 3.279552568209080290E-17, -0.8150194905431714654, 0.5794335423797530860 ) ) ;
#5660 = DIRECTION ( 'NONE',  ( 1.000000000000000000, 1.874307916738609066E-16, 0.000000000000000000 ) ) ;
#5661 = VERTEX_POINT ( 'NONE', #6148 ) ;
#5662 = CARTESIAN_POINT ( 'NONE',  ( 0.4125000000000000333, 0.1749999999999999889, 0.3724999999999999978 ) ) ;
#5663 = DIRECTION ( 'NONE',  ( 0.9396926207859107594, 0.000000000000000000, -0.3420201433256624401 ) ) ;
#5664 = AXIS2_PLACEMENT_3D ( 'NONE', #10513, #9, #12553 ) ;
#5665 = PLANE ( 'NONE',  #14486 ) ;
#5666 = CARTESIAN_POINT ( 'NONE',  ( 0.6179999999999965521, 1.679378605318059492, 1.679378605318041506 ) ) ;
#5667 = CARTESIAN_POINT ( 'NONE',  ( 3.429441573760528161, -0.4329758086553958107, 0.5000000000000000000 ) ) ;
#5668 = DIRECTION ( 'NONE',  ( 0.000000000000000000, 0.000000000000000000, 1.000000000000000000 ) ) ;
#5669 = DIRECTION ( 'NONE',  ( 0.000000000000000000, 0.000000000000000000, 1.000000000000000000 ) ) ;
#5670 = CARTESIAN_POINT ( 'NONE',  ( 3.407667229351369009, 0.9840573826600637064, -0.1785091600307283921 ) ) ;
#5671 = CARTESIAN_POINT ( 'NONE',  ( 3.716778723645624449, 1.830546595533379950, -0.7880236670140078337 ) ) ;
#5672 = VECTOR ( 'NONE', #11045, 39.37007874015748143 ) ;
#5673 = CARTESIAN_POINT ( 'NONE',  ( 6.176491571325181340, -1.679378605318048390, 2.086378605318056412 ) ) ;
#5675 = VERTEX_POINT ( 'NONE', #1308 ) ;
#5674 = DIRECTION ( 'NONE',  ( 1.000000000000000000, 0.000000000000000000, 0.000000000000000000 ) ) ;
#5676 = ORIENTED_EDGE ( 'NONE', *, *, #9360, .T. ) ;
#5677 = DIRECTION ( 'NONE',  ( 0.000000000000000000, -1.000000000000000000, 0.000000000000000000 ) ) ;
#5678 = EDGE_LOOP ( 'NONE', ( #10987, #7748, #7757, #12865 ) ) ;
#5679 = DIRECTION ( 'NONE',  ( 0.000000000000000000, -0.000000000000000000, 1.000000000000000000 ) ) ;
#5680 = CARTESIAN_POINT ( 'NONE',  ( 3.025735579118526974, 0.6832920890234898126, -0.4572636217638627043 ) ) ;
#5681 = EDGE_CURVE ( 'NONE', #10530, #9031, #5003, .T. ) ;
#5682 = EDGE_CURVE ( 'NONE', #13454, #4934, #4687, .T. ) ;
#5683 = CARTESIAN_POINT ( 'NONE',  ( 0.7010312871322603723, -0.4463509627415067071, -0.4267273516602834160 ) ) ;
#5684 = DIRECTION ( 'NONE',  ( -1.000000000000000000, -0.000000000000000000, -0.000000000000000000 ) ) ;
#5685 = EDGE_CURVE ( 'NONE', #327, #11008, #11764, .T. ) ;
#5686 = CARTESIAN_POINT ( 'NONE',  ( 0.9672769954795885639, -0.4829975555521403008, -0.4081482409674996870 ) ) ;
#5687 = ORIENTED_EDGE ( 'NONE', *, *, #9706, .F. ) ;
#5688 = CYLINDRICAL_SURFACE ( 'NONE', #1332, 0.4849999999999995981 ) ;
#5689 = CARTESIAN_POINT ( 'NONE',  ( 3.716337281397007253, 1.830387028050574738, 0.7888129363977544051 ) ) ;
#5690 = VERTEX_POINT ( 'NONE', #11504 ) ;
#5691 = EDGE_CURVE ( 'NONE', #11839, #5850, #14010, .T. ) ;
#5692 = CARTESIAN_POINT ( 'NONE',  ( 0.3724999999999999423, 0.1859999999999983611, 0.3724999999999999423 ) ) ;
#5693 = VERTEX_POINT ( 'NONE', #925 ) ;
#5694 = CARTESIAN_POINT ( 'NONE',  ( 3.394491571325180423, -1.679378605318059048, -1.941878605318027251 ) ) ;
#5695 = AXIS2_PLACEMENT_3D ( 'NONE', #15089, #5991, #4620 ) ;
#5696 = DIRECTION ( 'NONE',  ( 0.000000000000000000, 0.000000000000000000, 1.000000000000000000 ) ) ;
#5697 = VERTEX_POINT ( 'NONE', #4544 ) ;
#5698 = CARTESIAN_POINT ( 'NONE',  ( 3.319863249854034581, 0.6888833692903483241, 0.3931858364370117709 ) ) ;
#5699 = CARTESIAN_POINT ( 'NONE',  ( 4.769268701363833074, 3.567999999999999616, 0.3249191361593796734 ) ) ;
#5700 = CARTESIAN_POINT ( 'NONE',  ( 0.8359884731686543224, -0.4372643507807087992, -0.4540055247929744575 ) ) ;
#5701 = DIRECTION ( 'NONE',  ( -1.000000000000000000, -0.000000000000000000, -0.000000000000000000 ) ) ;
#5702 = CARTESIAN_POINT ( 'NONE',  ( 0.000000000000000000, 0.1749999999999999889, 0.000000000000000000 ) ) ;
#5703 =( BOUNDED_SURFACE ( )  B_SPLINE_SURFACE ( 3, 2, ( 
 ( #13728, #6946, #11683 ),
 ( #10379, #6792, #5718 ),
 ( #13957, #12580, #2106 ),
 ( #13804, #3263, #12664 ),
 ( #3494, #7933, #10456 ),
 ( #15043, #14967, #4571 ),
 ( #3338, #8097, #13878 ),
 ( #2025, #4648, #11451 ),
 ( #4489, #9160, #6874 ),
 ( #15117, #3421, #5647 ),
 ( #2190, #9238, #3196 ),
 ( #4422, #14815, #1106 ),
 ( #10306, #8014, #12738 ),
 ( #13661, #11527, #2263 ) ),
 .UNSPECIFIED., .F., .F., .T. ) 
 B_SPLINE_SURFACE_WITH_KNOTS ( ( 4, 2, 2, 2, 2, 2, 4 ),
 ( 3, 3 ),
 ( 0.001551397270042531020, 0.002805300020215382474, 0.004059202770388233711, 0.004686154145474659763, 0.005313105520561085815, 0.005940056895647511867, 0.006567008270733937052 ),
 ( 0.000000000000000000, 1.000000000000000000 ),
 .UNSPECIFIED. ) 
 GEOMETRIC_REPRESENTATION_ITEM ( )  RATIONAL_B_SPLINE_SURFACE ( (
 ( 1.000000000000000000, 0.8091170061680381664, 1.000000000000000000),
 ( 1.000000000000000000, 0.8270513381945645559, 1.000000000000000000),
 ( 1.000000000000000000, 0.8430705034768221084, 1.000000000000000000),
 ( 1.000000000000000000, 0.8715016528490074910, 1.000000000000000000),
 ( 1.000000000000000000, 0.8830758126916298245, 1.000000000000000000),
 ( 1.000000000000000000, 0.8962350306362059094, 1.000000000000000000),
 ( 1.000000000000000000, 0.8997443014200150468, 1.000000000000000000),
 ( 1.000000000000000000, 0.9049100909109204505, 1.000000000000000000),
 ( 1.000000000000000000, 0.9065649576647841767, 1.000000000000000000),
 ( 1.000000000000000000, 0.9077684922225311981, 1.000000000000000000),
 ( 1.000000000000000000, 0.9073563424325319371, 1.000000000000000000),
 ( 1.000000000000000000, 0.9044691270900298008, 1.000000000000000000),
 ( 1.000000000000000000, 0.9020443801113525728, 1.000000000000000000),
 ( 1.000000000000000000, 0.8987017906623396835, 1.000000000000000000) ) ) 
 REPRESENTATION_ITEM ( '' )  SURFACE ( )  );
#5704 = AXIS2_PLACEMENT_3D ( 'NONE', #13666, #2970, #4273 ) ;
#5705 = CARTESIAN_POINT ( 'NONE',  ( 3.894800534755237909, 1.849893891846735139, -0.7499754145434819330 ) ) ;
#5706 = VERTEX_POINT ( 'NONE', #5694 ) ;
#5707 = ORIENTED_EDGE ( 'NONE', *, *, #6878, .T. ) ;
#5708 = EDGE_CURVE ( 'NONE', #4450, #14996, #10297, .T. ) ;
#5709 = CARTESIAN_POINT ( 'NONE',  ( 3.389333715882079101, 0.6913093314209972640, 0.3921516461332968939 ) ) ;
#5710 = VERTEX_POINT ( 'NONE', #12787 ) ;
#5711 = DIRECTION ( 'NONE',  ( -0.000000000000000000, 1.000000000000000000, 0.000000000000000000 ) ) ;
#5712 = CARTESIAN_POINT ( 'NONE',  ( 2.527624975756972425, 3.137999999999999901, 0.9199802545633498640 ) ) ;
#5713 = CARTESIAN_POINT ( 'NONE',  ( 0.8051298376193415374, -0.4429999999999779670, -0.3049516186061956291 ) ) ;
#5714 = EDGE_CURVE ( 'NONE', #616, #12557, #13455, .T. ) ;
#5715 = CARTESIAN_POINT ( 'NONE',  ( -0.1950126918253222708, 1.569501570604565632, 0.3809527529760086129 ) ) ;
#5716 = ORIENTED_EDGE ( 'NONE', *, *, #14111, .F. ) ;
#5717 = DIRECTION ( 'NONE',  ( -0.7071067811865441310, 8.659560562354974766E-17, -0.7071067811865509034 ) ) ;
#5718 = CARTESIAN_POINT ( 'NONE',  ( 0.7429169091363049260, -3.303005800603283850E-18, -0.4367090053325354271 ) ) ;
#5719 = AXIS2_PLACEMENT_3D ( 'NONE', #8277, #8355, #200 ) ;
#5720 = CARTESIAN_POINT ( 'NONE',  ( 0.2249147617188371751, 0.7512260236060024354, -0.3723417112827391295 ) ) ;
#5721 = AXIS2_PLACEMENT_3D ( 'NONE', #5526, #14924, #2058 ) ;
#5722 = FILL_AREA_STYLE ('',( #1032 ) ) ;
#5723 = CARTESIAN_POINT ( 'NONE',  ( 4.605814143324980847, 1.746023016917476633, 0.1761007706937262884 ) ) ;
#5724 = ORIENTED_EDGE ( 'NONE', *, *, #10119, .T. ) ;
#5726 = ORIENTED_EDGE ( 'NONE', *, *, #12761, .T. ) ;
#5725 = DIRECTION ( 'NONE',  ( -1.000000000000000000, -0.000000000000000000, -0.000000000000000000 ) ) ;
#5727 = EDGE_LOOP ( 'NONE', ( #1407, #5274, #11590, #1469 ) ) ;
#5728 = AXIS2_PLACEMENT_3D ( 'NONE', #6194, #12073, #4979 ) ;
#5730 = VERTEX_POINT ( 'NONE', #8074 ) ;
#5729 = DIRECTION ( 'NONE',  ( -0.000000000000000000, 1.000000000000000000, -0.000000000000000000 ) ) ;
#5731 = ORIENTED_EDGE ( 'NONE', *, *, #14562, .T. ) ;
#5732 = LINE ( 'NONE', #10397, #2368 ) ;
#5733 = EDGE_CURVE ( 'NONE', #2357, #2874, #9077, .T. ) ;
#5734 =( CONVERSION_BASED_UNIT ( 'INCH', #1123 ) LENGTH_UNIT ( ) NAMED_UNIT ( #5305 ) );
#5735 = DIRECTION ( 'NONE',  ( -1.874307916738608820E-16, 1.000000000000000000, 0.000000000000000000 ) ) ;
#5736 = ORIENTED_EDGE ( 'NONE', *, *, #8783, .T. ) ;
#5737 = CARTESIAN_POINT ( 'NONE',  ( 2.807000000000000828, 1.679378605318042395, -1.679378605318058604 ) ) ;
#5738 = CARTESIAN_POINT ( 'NONE',  ( 4.315797241329101475, 3.137999999999999901, -1.570821732971949825 ) ) ;
#5739 = DIRECTION ( 'NONE',  ( 0.000000000000000000, -1.000000000000000000, 0.000000000000000000 ) ) ;
#5740 = LINE ( 'NONE', #12526, #9395 ) ;
#5741 = CARTESIAN_POINT ( 'NONE',  ( 8.476283996537762988, 0.8689495495877206377, 0.3203020658980471613 ) ) ;
#5742 = CARTESIAN_POINT ( 'NONE',  ( 3.876560711617219379, 2.749999999999999556, 0.000000000000000000 ) ) ;
#5743 = DIRECTION ( 'NONE',  ( 1.000000000000000000, 0.000000000000000000, 0.000000000000000000 ) ) ;
#5744 = CARTESIAN_POINT ( 'NONE',  ( 3.426755384177574193, 0.9750879638133824745, 0.2239670995506589934 ) ) ;
#5745 = CARTESIAN_POINT ( 'NONE',  ( 4.204541317192457051, 1.715952400129281630, 0.7235892913703009244 ) ) ;
#5746 = DIRECTION ( 'NONE',  ( -1.000000000000000000, -0.000000000000000000, -0.000000000000000000 ) ) ;
#5747 = PLANE ( 'NONE',  #9929 ) ;
#5748 = EDGE_LOOP ( 'NONE', ( #15028, #2509, #296, #2532 ) ) ;
#5749 = CONICAL_SURFACE ( 'NONE', #7692, 0.2219999999999999751, 0.7853981633974435050 ) ;
#5750 = CARTESIAN_POINT ( 'NONE',  ( 1.000847373107698779, -0.3829999999999998961, -0.4858637376679703634 ) ) ;
#5751 = ORIENTED_EDGE ( 'NONE', *, *, #9735, .T. ) ;
#5752 = PLANE ( 'NONE',  #12196 ) ;
#5753 = CIRCLE ( 'NONE', #12085, 0.05999999999999995615 ) ;
#5754 = AXIS2_PLACEMENT_3D ( 'NONE', #12774, #3696, #2387 ) ;
#5755 = DIRECTION ( 'NONE',  ( -1.000000000000000000, -0.000000000000000000, -0.000000000000000000 ) ) ;
#5756 = CARTESIAN_POINT ( 'NONE',  ( 1.645138957953503622, -0.3406142803323702895, 0.4767635740404712053 ) ) ;
#5757 = LINE ( 'NONE', #13621, #8013 ) ;
#5758 = CARTESIAN_POINT ( 'NONE',  ( 2.774999999999999911, 2.400000000000010569, 0.6999999999999612088 ) ) ;
#5759 = EDGE_LOOP ( 'NONE', ( #10745, #11076, #14309, #13705 ) ) ;
#5760 = CARTESIAN_POINT ( 'NONE',  ( 0.6729652567417304665, -0.4032054944085891601, 0.4872362964973896982 ) ) ;
#5761 = DIRECTION ( 'NONE',  ( 0.01412288512831583534, 0.000000000000000000, 0.9999002670844989726 ) ) ;
#5762 = CIRCLE ( 'NONE', #11626, 0.4999999999999995004 ) ;
#5763 = AXIS2_PLACEMENT_3D ( 'NONE', #6277, #13067, #13143 ) ;
#5764 = ORIENTED_EDGE ( 'NONE', *, *, #7399, .F. ) ;
#5765 = LINE ( 'NONE', #2075, #9912 ) ;
#5766 = EDGE_LOOP ( 'NONE', ( #13849, #486, #5, #9361 ) ) ;
#5767 = EDGE_CURVE ( 'NONE', #13629, #11914, #14864, .T. ) ;
#5768 = CARTESIAN_POINT ( 'NONE',  ( 0.6500000000000001332, -1.679378605318048390, 1.272378605318049249 ) ) ;
#5769 = ORIENTED_EDGE ( 'NONE', *, *, #8994, .F. ) ;
#5770 = ADVANCED_FACE ( 'NONE', ( #9133 ), #2241, .F. ) ;
#5771 = PLANE ( 'NONE',  #5510 ) ;
#5772 = AXIS2_PLACEMENT_3D ( 'NONE', #8363, #7057, #13991 ) ;
#5773 = CARTESIAN_POINT ( 'NONE',  ( 1.645138957954975778, -0.3406142803326386859, -0.4767635740401386935 ) ) ;
#5774 = CIRCLE ( 'NONE', #14313, 0.4070000000000058016 ) ;
#5775 = CIRCLE ( 'NONE', #6750, 1.000000000000000000 ) ;
#5776 = EDGE_CURVE ( 'NONE', #2606, #10222, #9321, .T. ) ;
#5777 = DIRECTION ( 'NONE',  ( -1.000000000000000000, -0.000000000000000000, -0.000000000000000000 ) ) ;
#5778 = CARTESIAN_POINT ( 'NONE',  ( 0.06299999999999994493, -1.679378605318047946, -1.679378605318053497 ) ) ;
#5779 = AXIS2_PLACEMENT_3D ( 'NONE', #14129, #13966, #4731 ) ;
#5780 = ORIENTED_EDGE ( 'NONE', *, *, #1553, .T. ) ;
#5781 = EDGE_CURVE ( 'NONE', #3137, #947, #10053, .T. ) ;
#5782 = ORIENTED_EDGE ( 'NONE', *, *, #4248, .F. ) ;
#5783 = DIRECTION ( 'NONE',  ( 0.000000000000000000, 0.000000000000000000, -1.000000000000000000 ) ) ;
#5784 = ORIENTED_EDGE ( 'NONE', *, *, #3342, .T. ) ;
#5785 = EDGE_CURVE ( 'NONE', #6053, #10522, #2965, .T. ) ;
#5786 = DIRECTION ( 'NONE',  ( 0.000000000000000000, 0.000000000000000000, 1.000000000000000000 ) ) ;
#5787 = LINE ( 'NONE', #2568, #12987 ) ;
#5788 = CARTESIAN_POINT ( 'NONE',  ( -0.3725000000000000533, 0.2159999999999999420, 0.4425000000000003930 ) ) ;
#5789 = CARTESIAN_POINT ( 'NONE',  ( 3.874999999999999556, 3.137999999999999901, 1.320000000000000062 ) ) ;
#5790 = EDGE_LOOP ( 'NONE', ( #8170, #14456 ) ) ;
#5791 = CARTESIAN_POINT ( 'NONE',  ( 3.381088951121218766, 2.435687008709748635, -0.5637784091204912640 ) ) ;
#5792 = AXIS2_PLACEMENT_3D ( 'NONE', #173, #11594, #10450 ) ;
#5793 = CARTESIAN_POINT ( 'NONE',  ( 2.591520038054473840, 0.4049457270506677253, 0.4033906250602100618 ) ) ;
#5794 =( BOUNDED_CURVE ( )  B_SPLINE_CURVE ( 3, ( #2699, #4999, #9803, #13225 ),
 .UNSPECIFIED., .F., .F. ) 
 B_SPLINE_CURVE_WITH_KNOTS ( ( 4, 4 ),
 ( 1.572344395910955761, 2.356194490192339952 ),
 .UNSPECIFIED. ) 
 CURVE ( )  GEOMETRIC_REPRESENTATION_ITEM ( )  RATIONAL_B_SPLINE_CURVE ( ( 1.000000000000000000, 0.9494503106142797577, 0.9494503106142797577, 1.000000000000000000 ) ) 
 REPRESENTATION_ITEM ( '' )  );
#5795 = DIRECTION ( 'NONE',  ( 1.000000000000000000, 0.000000000000000000, 0.000000000000000000 ) ) ;
#5796 = EDGE_CURVE ( 'NONE', #8103, #15092, #574, .T. ) ;
#5797 = CIRCLE ( 'NONE', #11434, 1.039370078740158965 ) ;
#5798 = CARTESIAN_POINT ( 'NONE',  ( 2.774999999999999911, 0.6999999999999599876, -2.400000000000011458 ) ) ;
#5799 = ADVANCED_FACE ( 'NONE', ( #9525 ), #5568, .F. ) ;
#5800 = CARTESIAN_POINT ( 'NONE',  ( 4.623877826222967613, 1.809988068179393395, 0.07275869780465363257 ) ) ;
#5801 = ORIENTED_EDGE ( 'NONE', *, *, #4700, .T. ) ;
#5803 = ORIENTED_EDGE ( 'NONE', *, *, #12432, .F. ) ;
#5802 = PLANE ( 'NONE',  #11569 ) ;
#5804 = VECTOR ( 'NONE', #11044, 39.37007874015748143 ) ;
#5805 = VERTEX_POINT ( 'NONE', #3731 ) ;
#5807 = ORIENTED_EDGE ( 'NONE', *, *, #5610, .T. ) ;
#5806 = DIRECTION ( 'NONE',  ( -0.7071067811865400232, 8.659560562355026535E-17, -0.7071067811865551223 ) ) ;
#5808 = ORIENTED_EDGE ( 'NONE', *, *, #7281, .F. ) ;
#5809 = FACE_OUTER_BOUND ( 'NONE', #14169, .T. ) ;
#5810 = CARTESIAN_POINT ( 'NONE',  ( 3.234999999999999876, -1.679378605318059714, -1.679378605318042395 ) ) ;
#5811 = FACE_BOUND ( 'NONE', #12824, .T. ) ;
#5812 = EDGE_LOOP ( 'NONE', ( #8391, #13291, #1389, #4205 ) ) ;
#5813 = LINE ( 'NONE', #12601, #11414 ) ;
#5814 = CARTESIAN_POINT ( 'NONE',  ( 2.045495128834867504, 0.3295048711651357154, 0.5000000000000000000 ) ) ;
#5815 = CIRCLE ( 'NONE', #4835, 1.932031071636253650 ) ;
#5816 = EDGE_CURVE ( 'NONE', #7551, #7156, #1242, .T. ) ;
#5817 = CARTESIAN_POINT ( 'NONE',  ( 8.849999999999999645, -0.4430000000000001714, 0.3750000000000000555 ) ) ;
#5818 = CARTESIAN_POINT ( 'NONE',  ( 3.394491571325182644, 1.679378605318042395, -1.416878605318058870 ) ) ;
#5819 = B_SPLINE_CURVE_WITH_KNOTS ( 'NONE', 3,
 ( #12742, #11836, #9478, #35, #7034, #2438, #4728, #6029, #13888, #10463, #3347, #9402, #14125, #3498, #6952, #4654, #3424, #2269, #3665, #12821, #10541, #1339 ),
 .UNSPECIFIED., .F., .F.,
 ( 4, 2, 2, 2, 2, 2, 2, 2, 2, 2, 4 ),
 ( 2.884201054326571187E-07, 0.0006930185370334598005, 0.001385748653961486974, 0.002771208887817543706, 0.004156669121673600004, 0.005542129355529658470, 0.006927589589385716069, 0.008313049823241772801, 0.009698510057097830400, 0.01039124017402585226, 0.01108397029095387412 ),
 .UNSPECIFIED. ) ;
#5820 = CARTESIAN_POINT ( 'NONE',  ( 0.000000000000000000, 1.866025403784438819, 0.000000000000000000 ) ) ;
#5821 = AXIS2_PLACEMENT_3D ( 'NONE', #7091, #6084, #86 ) ;
#5822 = DIRECTION ( 'NONE',  ( 0.000000000000000000, 0.000000000000000000, -1.000000000000000000 ) ) ;
#5823 = ADVANCED_FACE ( 'NONE', ( #1414 ), #2433, .F. ) ;
#5824 = LINE ( 'NONE', #9187, #6083 ) ;
#5825 = DIRECTION ( 'NONE',  ( 0.000000000000000000, 0.000000000000000000, -1.000000000000000000 ) ) ;
#5826 = CIRCLE ( 'NONE', #9489, 0.07500000000000002498 ) ;
#5827 = CARTESIAN_POINT ( 'NONE',  ( 4.657066280160475635, 1.728587765848446089, 0.2078677355136313021 ) ) ;
#5828 = VERTEX_POINT ( 'NONE', #7180 ) ;
#5829 = CARTESIAN_POINT ( 'NONE',  ( 0.1250000000000009992, 0.000000000000000000, 0.000000000000000000 ) ) ;
#5831 = EDGE_LOOP ( 'NONE', ( #14045, #4449, #90, #4008 ) ) ;
#5830 = DIRECTION ( 'NONE',  ( -1.000000000000000000, 0.000000000000000000, 0.000000000000000000 ) ) ;
#5832 = ORIENTED_EDGE ( 'NONE', *, *, #9098, .T. ) ;
#5833 = DIRECTION ( 'NONE',  ( 8.659560562354973534E-17, 0.7071067811865441310, -0.7071067811865509034 ) ) ;
#5834 = CARTESIAN_POINT ( 'NONE',  ( 0.6566521509169384041, -0.01162981109769697236, -0.4973154343666586485 ) ) ;
#5835 = VERTEX_POINT ( 'NONE', #10832 ) ;
#5836 = CONICAL_SURFACE ( 'NONE', #12174, 0.08500000000000004774, 0.7853981633974541632 ) ;
#5837 = DIRECTION ( 'NONE',  ( -0.000000000000000000, -1.000000000000000000, -0.000000000000000000 ) ) ;
#5838 = CIRCLE ( 'NONE', #9749, 0.8083085967350902568 ) ;
#5839 = ADVANCED_BREP_SHAPE_REPRESENTATION ( '', ( #5616, #8424 ), #10848 ) ;
#5840 = CARTESIAN_POINT ( 'NONE',  ( 5.939536975864663462E-17, 0.000000000000000000, 0.4850000000000000422 ) ) ;
#5841 = AXIS2_PLACEMENT_3D ( 'NONE', #13311, #14776, #3167 ) ;
#5842 = VECTOR ( 'NONE', #6824, 39.37007874015748143 ) ;
#5843 = LINE ( 'NONE', #2150, #6324 ) ;
#5844 = ORIENTED_EDGE ( 'NONE', *, *, #5627, .F. ) ;
#5845 = ADVANCED_FACE ( 'NONE', ( #5102 ), #3212, .F. ) ;
#5846 = AXIS2_PLACEMENT_3D ( 'NONE', #6296, #13376, #10954 ) ;
#5847 = CARTESIAN_POINT ( 'NONE',  ( 0.6610203958102930377, -0.4494184719130550065, 0.4833908188384043458 ) ) ;
#5848 = DIRECTION ( 'NONE',  ( 0.9999002670844991947, 0.000000000000000000, -0.01412288512831213171 ) ) ;
#5849 = DIRECTION ( 'NONE',  ( 0.000000000000000000, 0.000000000000000000, -1.000000000000000000 ) ) ;
#5850 = VERTEX_POINT ( 'NONE', #1335 ) ;
#5851 = CIRCLE ( 'NONE', #10971, 1.875000000000000000 ) ;
#5852 = CARTESIAN_POINT ( 'NONE',  ( 4.344846310392954436, 3.137999999999999901, -1.491010071662831171 ) ) ;
#5853 = EDGE_LOOP ( 'NONE', ( #9629, #14220, #1873, #4581 ) ) ;
#5854 = DIRECTION ( 'NONE',  ( 0.000000000000000000, 0.000000000000000000, 1.000000000000000000 ) ) ;
#5855 = CARTESIAN_POINT ( 'NONE',  ( 6.176491571325181340, 1.679378605318059492, 2.086378605318043533 ) ) ;
#5856 = EDGE_LOOP ( 'NONE', ( #9060, #8502, #14024, #8446 ) ) ;
#5857 = FACE_OUTER_BOUND ( 'NONE', #12567, .T. ) ;
#5858 = TOROIDAL_SURFACE ( 'NONE', #3659, 0.0001794190581142465670, 1.999999999999999334 ) ;
#5859 = CARTESIAN_POINT ( 'NONE',  ( 1.000847373107695226, -0.3830000000000000071, -0.4858637376679705855 ) ) ;
#5860 = CIRCLE ( 'NONE', #2923, 0.3750000000000004996 ) ;
#5861 = DIRECTION ( 'NONE',  ( -1.000000000000000000, -0.000000000000000000, -0.000000000000000000 ) ) ;
#5862 = DIRECTION ( 'NONE',  ( -1.874307916738606601E-16, 1.000000000000000000, 0.000000000000000000 ) ) ;
#5863 = AXIS2_PLACEMENT_3D ( 'NONE', #10570, #15080, #3379 ) ;
#5864 = CARTESIAN_POINT ( 'NONE',  ( 4.016777269453733368, 1.816382256245877569, -0.7376231757443032500 ) ) ;
#5865 = ORIENTED_EDGE ( 'NONE', *, *, #11018, .T. ) ;
#5866 = EDGE_LOOP ( 'NONE', ( #11344, #10974, #8620, #14954 ) ) ;
#5867 = CIRCLE ( 'NONE', #6123, 0.4849999999999995981 ) ;
#5868 = CARTESIAN_POINT ( 'NONE',  ( 3.426491571325181340, 2.062169880637645836, 0.5999481385559802815 ) ) ;
#5869 = ORIENTED_EDGE ( 'NONE', *, *, #2773, .T. ) ;
#5870 = CARTESIAN_POINT ( 'NONE',  ( 0.3932619838308991644, 1.593633255602470156, -0.08075576927157292195 ) ) ;
#5871 = CARTESIAN_POINT ( 'NONE',  ( 1.522243911113194015, -0.3830000000000001181, 0.4784993797865367826 ) ) ;
#5872 = CARTESIAN_POINT ( 'NONE',  ( -0.2099999999999999922, 0.7512260236060024354, -0.3809527529760087239 ) ) ;
#5873 = CARTESIAN_POINT ( 'NONE',  ( 2.774999999999999911, 0.000000000000000000, 0.000000000000000000 ) ) ;
#5874 = ORIENTED_EDGE ( 'NONE', *, *, #11032, .T. ) ;
#5875 = CARTESIAN_POINT ( 'NONE',  ( 0.8083085967350902568, 0.04143956043956045082, 0.000000000000000000 ) ) ;
#5876 = DIRECTION ( 'NONE',  ( -0.000000000000000000, -1.000000000000000000, -0.000000000000000000 ) ) ;
#5877 = CARTESIAN_POINT ( 'NONE',  ( -0.3725000000000000533, 0.2159999999999999698, 0.4124999999999999223 ) ) ;
#5878 = EDGE_CURVE ( 'NONE', #557, #2828, #14937, .T. ) ;
#5879 = CONICAL_SURFACE ( 'NONE', #3921, 0.1899999999999996136, 0.7853981633974433940 ) ;
#5880 = ADVANCED_FACE ( 'NONE', ( #8474 ), #999, .F. ) ;
#5881 = EDGE_CURVE ( 'NONE', #4965, #3991, #11266, .T. ) ;
#5882 = DIRECTION ( 'NONE',  ( 0.000000000000000000, 0.000000000000000000, -1.000000000000000000 ) ) ;
#5883 = CARTESIAN_POINT ( 'NONE',  ( 4.626593255961919837, 1.749179356862341939, -0.01614418902847078105 ) ) ;
#5884 = VERTEX_POINT ( 'NONE', #11128 ) ;
#5886 = VERTEX_POINT ( 'NONE', #4098 ) ;
#5885 = FACE_OUTER_BOUND ( 'NONE', #3754, .T. ) ;
#5887 = ADVANCED_FACE ( 'NONE', ( #4252 ), #12272, .T. ) ;
#5888 = EDGE_CURVE ( 'NONE', #14656, #10542, #3456, .T. ) ;
#5889 = VERTEX_POINT ( 'NONE', #4019 ) ;
#5890 = LINE ( 'NONE', #12745, #2105 ) ;
#5891 = VERTEX_POINT ( 'NONE', #7468 ) ;
#5892 = DIRECTION ( 'NONE',  ( -1.000000000000000000, -0.000000000000000000, -0.000000000000000000 ) ) ;
#5893 = DIRECTION ( 'NONE',  ( 0.03462124711963855683, 3.313444278808240493E-16, -0.9994005049267692398 ) ) ;
#5894 = DIRECTION ( 'NONE',  ( 0.000000000000000000, 0.000000000000000000, 1.000000000000000000 ) ) ;
#5895 = ORIENTED_EDGE ( 'NONE', *, *, #4844, .F. ) ;
#5896 = CARTESIAN_POINT ( 'NONE',  ( 0.000000000000000000, 1.603403463250997918, -0.3809527529760087239 ) ) ;
#5897 = CARTESIAN_POINT ( 'NONE',  ( 2.774999999999999911, 0.000000000000000000, 2.500000000000000444 ) ) ;
#5898 = DIRECTION ( 'NONE',  ( 0.7071067811865336949, 0.7071067811865612285, 0.000000000000000000 ) ) ;
#5899 = CARTESIAN_POINT ( 'NONE',  ( 3.944129661530210385, 1.867491090171841117, 0.4951980309903491473 ) ) ;
#5900 = TOROIDAL_SURFACE ( 'NONE', #11258, 1.580000000000000071, 0.08000000000000000167 ) ;
#5901 = DIRECTION ( 'NONE',  ( 8.659560562354890950E-17, -0.7071067811865509034, 0.7071067811865441310 ) ) ;
#5902 = ORIENTED_EDGE ( 'NONE', *, *, #9222, .F. ) ;
#5903 = CARTESIAN_POINT ( 'NONE',  ( 3.759965575530244131, 0.8734814492854425794, 0.4868720398751328893 ) ) ;
#5904 = CARTESIAN_POINT ( 'NONE',  ( 4.661486646721258786, 1.729257228445998384, -0.1974800237815390325 ) ) ;
#5905 = ORIENTED_EDGE ( 'NONE', *, *, #5781, .T. ) ;
#5906 = DIRECTION ( 'NONE',  ( 0.000000000000000000, 0.000000000000000000, 1.000000000000000000 ) ) ;
#5908 = ORIENTED_EDGE ( 'NONE', *, *, #7113, .F. ) ;
#5907 = CARTESIAN_POINT ( 'NONE',  ( 0.6569077226922027668, -0.4429999999999999494, 0.4307156577630670280 ) ) ;
#5909 = ORIENTED_EDGE ( 'NONE', *, *, #7003, .F. ) ;
#5910 = EDGE_CURVE ( 'NONE', #7869, #251, #13415, .T. ) ;
#5911 = DIRECTION ( 'NONE',  ( -0.000000000000000000, -1.000000000000000000, -0.000000000000000000 ) ) ;
#5912 = ORIENTED_EDGE ( 'NONE', *, *, #13754, .F. ) ;
#5913 = DIRECTION ( 'NONE',  ( 1.000000000000000000, 0.000000000000000000, 0.000000000000000000 ) ) ;
#5914 = ADVANCED_FACE ( 'NONE', ( #10984 ), #6396, .F. ) ;
#5915 = LINE ( 'NONE', #9588, #13535 ) ;
#5916 = CARTESIAN_POINT ( 'NONE',  ( 8.475037399843312613, 0.8689060174719044349, -0.3802960819231170908 ) ) ;
#5917 = VERTEX_POINT ( 'NONE', #938 ) ;
#5918 = CARTESIAN_POINT ( 'NONE',  ( 3.551656769079091003, 1.993509976604513234, -0.6761768950259927635 ) ) ;
#5919 = VECTOR ( 'NONE', #3649, 39.37007874015748143 ) ;
#5920 = DIRECTION ( 'NONE',  ( 0.000000000000000000, 0.000000000000000000, -1.000000000000000000 ) ) ;
#5921 = DIRECTION ( 'NONE',  ( 0.000000000000000000, 0.000000000000000000, 1.000000000000000000 ) ) ;
#5922 = ORIENTED_EDGE ( 'NONE', *, *, #6913, .F. ) ;
#5923 = DIRECTION ( 'NONE',  ( 0.000000000000000000, 1.000000000000000000, 0.000000000000000000 ) ) ;
#5924 = ORIENTED_EDGE ( 'NONE', *, *, #7838, .T. ) ;
#5925 = CARTESIAN_POINT ( 'NONE',  ( 0.7513246802501660770, 0.000000000000000000, 0.4293820849162031661 ) ) ;
#5926 = ORIENTED_EDGE ( 'NONE', *, *, #2912, .T. ) ;
#5927 = CARTESIAN_POINT ( 'NONE',  ( 0.6412116890856961460, -0.6589999999999996971, 7.852578426146655751E-17 ) ) ;
#5928 = ADVANCED_FACE ( 'NONE', ( #9000 ), #14688, .F. ) ;
#5929 = FACE_OUTER_BOUND ( 'NONE', #3868, .T. ) ;
#5930 = CARTESIAN_POINT ( 'NONE',  ( 0.09500000000000431710, -1.679378605318048390, 1.679378605318054163 ) ) ;
#5931 = DIRECTION ( 'NONE',  ( 0.000000000000000000, 0.000000000000000000, -1.000000000000000000 ) ) ;
#5932 = AXIS2_PLACEMENT_3D ( 'NONE', #3, #14167, #4695 ) ;
#5933 = EDGE_LOOP ( 'NONE', ( #4127, #11096, #10229, #5335, #12747, #3054 ) ) ;
#5934 = ORIENTED_EDGE ( 'NONE', *, *, #5015, .T. ) ;
#5935 = DIRECTION ( 'NONE',  ( 0.000000000000000000, 0.000000000000000000, -1.000000000000000000 ) ) ;
#5936 = DIRECTION ( 'NONE',  ( 0.000000000000000000, 0.000000000000000000, 1.000000000000000000 ) ) ;
#5937 = AXIS2_PLACEMENT_3D ( 'NONE', #12444, #14817, #1960 ) ;
#5938 = CARTESIAN_POINT ( 'NONE',  ( 0.8553300727722267238, -0.4749930492489788381, -0.4355902931210492435 ) ) ;
#5939 = DIRECTION ( 'NONE',  ( -0.7071067811865452413, 0.000000000000000000, 0.7071067811865496822 ) ) ;
#5940 = DIRECTION ( 'NONE',  ( -1.000000000000000000, -0.000000000000000000, -0.000000000000000000 ) ) ;
#5941 = ORIENTED_EDGE ( 'NONE', *, *, #2303, .T. ) ;
#5942 = EDGE_CURVE ( 'NONE', #1772, #11127, #12722, .T. ) ;
#5943 = CARTESIAN_POINT ( 'NONE',  ( 3.828954533788070602, 1.894954944681144449, -0.4980091310583387720 ) ) ;
#5944 = AXIS2_PLACEMENT_3D ( 'NONE', #957, #5569, #1112 ) ;
#5945 = CARTESIAN_POINT ( 'NONE',  ( 2.774999999999999911, 0.000000000000000000, 0.000000000000000000 ) ) ;
#5946 = DIRECTION ( 'NONE',  ( 0.000000000000000000, 1.000000000000000000, 0.000000000000000000 ) ) ;
#5947 = LINE ( 'NONE', #3937, #4721 ) ;
#5948 = CARTESIAN_POINT ( 'NONE',  ( 4.674335806064782162, 1.731351353581825681, 0.1332815962874349947 ) ) ;
#5949 = ORIENTED_EDGE ( 'NONE', *, *, #12761, .F. ) ;
#5951 = ORIENTED_EDGE ( 'NONE', *, *, #2880, .T. ) ;
#5950 = DIRECTION ( 'NONE',  ( -0.9659258262890699775, 0.000000000000000000, 0.2588190451025145222 ) ) ;
#5952 = ORIENTED_EDGE ( 'NONE', *, *, #14322, .F. ) ;
#5953 = DIRECTION ( 'NONE',  ( -0.7071067811865425767, 8.659560562354992023E-17, -0.7071067811865523467 ) ) ;
#5954 = ORIENTED_EDGE ( 'NONE', *, *, #15029, .T. ) ;
#5955 = EDGE_CURVE ( 'NONE', #8189, #8165, #3946, .T. ) ;
#5956 = ADVANCED_FACE ( 'NONE', ( #14879 ), #1378, .T. ) ;
#5957 = FACE_BOUND ( 'NONE', #5230, .T. ) ;
#5958 = DIRECTION ( 'NONE',  ( 5.551115123125782702E-17, -0.1854703866664282885, -0.9826498540527065506 ) ) ;
#5959 = CARTESIAN_POINT ( 'NONE',  ( 0.000000000000000000, 0.000000000000000000, 0.000000000000000000 ) ) ;
#5960 = ORIENTED_EDGE ( 'NONE', *, *, #13414, .F. ) ;
#5961 = EDGE_CURVE ( 'NONE', #4007, #906, #7192, .T. ) ;
#5962 = CIRCLE ( 'NONE', #2777, 0.4999999999999995004 ) ;
#5963 = DIRECTION ( 'NONE',  ( -0.000000000000000000, -1.000000000000000000, -0.000000000000000000 ) ) ;
#5964 = DIRECTION ( 'NONE',  ( -1.000000000000000000, -0.000000000000000000, -0.000000000000000000 ) ) ;
#5965 = DIRECTION ( 'NONE',  ( 0.000000000000000000, 0.000000000000000000, -1.000000000000000000 ) ) ;
#5966 = ADVANCED_FACE ( 'NONE', ( #10734 ), #4490, .F. ) ;
#5967 = DIRECTION ( 'NONE',  ( 0.000000000000000000, 0.000000000000000000, 1.000000000000000000 ) ) ;
#5968 = CARTESIAN_POINT ( 'NONE',  ( 1.375000000000000000, 0.000000000000000000, 0.000000000000000000 ) ) ;
#5969 = CIRCLE ( 'NONE', #15003, 0.2944999999999856066 ) ;
#5970 = DIRECTION ( 'NONE',  ( 0.000000000000000000, -1.000000000000000000, 0.000000000000000000 ) ) ;
#5971 = FACE_BOUND ( 'NONE', #13563, .T. ) ;
#5972 = CIRCLE ( 'NONE', #4254, 1.932031071636253650 ) ;
#5973 = ORIENTED_EDGE ( 'NONE', *, *, #14788, .F. ) ;
#5974 = CARTESIAN_POINT ( 'NONE',  ( 2.045495128834867060, 0.3295048711651353268, -0.4105035982572215469 ) ) ;
#5976 = ORIENTED_EDGE ( 'NONE', *, *, #8629, .T. ) ;
#5975 = DIRECTION ( 'NONE',  ( -0.9999002670844989726, -1.365787769249574676E-16, 0.01412288512831212997 ) ) ;
#5977 = ORIENTED_EDGE ( 'NONE', *, *, #10876, .T. ) ;
#5978 = EDGE_CURVE ( 'NONE', #4487, #10219, #11320, .T. ) ;
#5979 = CARTESIAN_POINT ( 'NONE',  ( 3.874999999999999556, 3.170500000000001428, -1.320000000000000062 ) ) ;
#5980 = CARTESIAN_POINT ( 'NONE',  ( 3.875000000000000000, 1.885381157978845312, 0.5000000000000002220 ) ) ;
#5981 = CARTESIAN_POINT ( 'NONE',  ( 2.644772327657329836, 0.4573506435455682584, 0.4626444586489077415 ) ) ;
#5982 = VERTEX_POINT ( 'NONE', #224 ) ;
#5983 = DIRECTION ( 'NONE',  ( -1.000000000000000000, -0.000000000000000000, -0.000000000000000000 ) ) ;
#5984 = CIRCLE ( 'NONE', #2561, 0.3750000000000004996 ) ;
#5985 = VECTOR ( 'NONE', #5347, 39.37007874015748143 ) ;
#5986 = CARTESIAN_POINT ( 'NONE',  ( 2.775039370078740131, -1.679378605318048390, 1.679378605318054163 ) ) ;
#5987 = CARTESIAN_POINT ( 'NONE',  ( 3.426491571325181340, 2.360000000000015863, 1.574999999999999956 ) ) ;
#5988 = EDGE_CURVE ( 'NONE', #4934, #6363, #4923, .T. ) ;
#5989 = ORIENTED_EDGE ( 'NONE', *, *, #10067, .F. ) ;
#5990 = CARTESIAN_POINT ( 'NONE',  ( 3.447264066911562619, 1.944154718373165780, -0.6966300195041605914 ) ) ;
#5991 = DIRECTION ( 'NONE',  ( -5.190764794801482736E-21, -1.000000000000000000, -3.675061474719450755E-19 ) ) ;
#5992 = DIRECTION ( 'NONE',  ( -1.000000000000000000, -0.000000000000000000, -0.000000000000000000 ) ) ;
#5993 = ORIENTED_EDGE ( 'NONE', *, *, #8516, .F. ) ;
#5994 = EDGE_CURVE ( 'NONE', #11113, #10545, #5962, .T. ) ;
#5995 = CARTESIAN_POINT ( 'NONE',  ( 3.405153689607044232, 3.137999999999999901, -1.491010071662831171 ) ) ;
#5996 = AXIS2_PLACEMENT_3D ( 'NONE', #7758, #768, #7907 ) ;
#5997 = CARTESIAN_POINT ( 'NONE',  ( 0.000000000000000000, 0.000000000000000000, -1.812500000000000222 ) ) ;
#5998 = ORIENTED_EDGE ( 'NONE', *, *, #4684, .F. ) ;
#5999 = AXIS2_PLACEMENT_3D ( 'NONE', #14349, #7476, #12061 ) ;
#6000 = DIRECTION ( 'NONE',  ( -1.000000000000000000, -0.000000000000000000, -0.000000000000000000 ) ) ;
#6001 = VERTEX_POINT ( 'NONE', #3064 ) ;
#6002 = DIRECTION ( 'NONE',  ( 0.000000000000000000, -1.000000000000000000, 4.591341165822166182E-16 ) ) ;
#6003 = CARTESIAN_POINT ( 'NONE',  ( 1.886302412727347999, -0.2406659208691243612, -0.4137268778527457558 ) ) ;
#6004 = CIRCLE ( 'NONE', #4036, 3.000000000000000444 ) ;
#6005 = FACE_OUTER_BOUND ( 'NONE', #11987, .T. ) ;
#6006 = AXIS2_PLACEMENT_3D ( 'NONE', #7087, #84, #4778 ) ;
#6007 = DIRECTION ( 'NONE',  ( 0.000000000000000000, 0.000000000000000000, 1.000000000000000000 ) ) ;
#6008 = EDGE_CURVE ( 'NONE', #7355, #13657, #5740, .T. ) ;
#6009 = ADVANCED_FACE ( 'NONE', ( #9415 ), #13824, .T. ) ;
#6010 = SURFACE_STYLE_FILL_AREA ( #7166 ) ;
#6011 = ORIENTED_EDGE ( 'NONE', *, *, #12876, .F. ) ;
#6012 = ORIENTED_EDGE ( 'NONE', *, *, #13463, .T. ) ;
#6013 = ORIENTED_EDGE ( 'NONE', *, *, #1856, .T. ) ;
#6014 = AXIS2_PLACEMENT_3D ( 'NONE', #6998, #10130, #14784 ) ;
#6015 = DIRECTION ( 'NONE',  ( -1.000000000000000000, -1.874307916738609066E-16, 0.000000000000000000 ) ) ;
#6016 = DIRECTION ( 'NONE',  ( -1.000000000000000000, -0.000000000000000000, -0.000000000000000000 ) ) ;
#6017 = TOROIDAL_SURFACE ( 'NONE', #13313, 0.0001794190581142465670, 1.999999999999999334 ) ;
#6018 = DIRECTION ( 'NONE',  ( 0.000000000000000000, 0.000000000000000000, 1.000000000000000000 ) ) ;
#6019 = CARTESIAN_POINT ( 'NONE',  ( 0.7023896125859220296, -0.05117280967830968585, -0.4896155492289063216 ) ) ;
#6020 = VERTEX_POINT ( 'NONE', #2210 ) ;
#6021 = CARTESIAN_POINT ( 'NONE',  ( 3.663085273664862029, 1.933817475710640998, -0.4530194878470137354 ) ) ;
#6022 = LINE ( 'NONE', #2727, #3405 ) ;
#6023 = CARTESIAN_POINT ( 'NONE',  ( 2.774999999999999911, -1.679378605318059048, -1.679378605318041950 ) ) ;
#6024 = B_SPLINE_CURVE_WITH_KNOTS ( 'NONE', 3,
 ( #11642, #13837, #3377, #11560, #1144, #15078, #4604, #5834, #6709, #3914, #8507, #8578, #8367, #4988 ),
 .UNSPECIFIED., .F., .F.,
 ( 4, 2, 2, 2, 2, 2, 4 ),
 ( 0.000000000000000000, 0.001176052134299114061, 0.002352104268598228121, 0.002940130335747782441, 0.003528156402897335894, 0.004116182470046890647, 0.004704208537196444967 ),
 .UNSPECIFIED. ) ;
#6025 = AXIS2_PLACEMENT_3D ( 'NONE', #7354, #12154, #7566 ) ;
#6026 = CARTESIAN_POINT ( 'NONE',  ( 1.541692889559683088, 0.03598127022577170264, -0.4179989611390685922 ) ) ;
#6027 = ADVANCED_FACE ( 'NONE', ( #14056, #1129 ), #5665, .F. ) ;
#6028 = ORIENTED_EDGE ( 'NONE', *, *, #241, .T. ) ;
#6030 = ORIENTED_EDGE ( 'NONE', *, *, #2904, .T. ) ;
#6029 = CARTESIAN_POINT ( 'NONE',  ( 0.3752176239131347346, 1.599166939805951593, 0.1120095174391954607 ) ) ;
#6031 = EDGE_LOOP ( 'NONE', ( #12042, #4429, #146, #8324, #9900, #10693, #13893, #14922, #7587, #5406, #7873 ) ) ;
#6032 = CARTESIAN_POINT ( 'NONE',  ( -0.09035531712817639061, 1.379999999999999671, -0.1564999999999998892 ) ) ;
#6033 = VERTEX_POINT ( 'NONE', #5818 ) ;
#6034 = FACE_BOUND ( 'NONE', #1072, .T. ) ;
#6035 = CONICAL_SURFACE ( 'NONE', #4320, 0.3750000000000004996, 0.7853981633974536081 ) ;
#6036 = DIRECTION ( 'NONE',  ( 1.000000000000000000, 0.000000000000000000, 0.000000000000000000 ) ) ;
#6037 = CARTESIAN_POINT ( 'NONE',  ( -0.1807106342563527812, 1.379999999999999671, 3.262375646219079751E-17 ) ) ;
#6038 = ORIENTED_EDGE ( 'NONE', *, *, #3869, .F. ) ;
#6039 = CARTESIAN_POINT ( 'NONE',  ( 0.9991526268923013321, -0.4429999999999998939, -0.4258816901896192997 ) ) ;
#6040 = CARTESIAN_POINT ( 'NONE',  ( -0.7287617923574205570, 0.2159999999999999420, -0.8499999999999999778 ) ) ;
#6041 = CARTESIAN_POINT ( 'NONE',  ( 0.3724999999999997757, 0.2159999999999999420, -0.4425000000000005596 ) ) ;
#6042 = VECTOR ( 'NONE', #2665, 39.37007874015748854 ) ;
#6043 = PRODUCT_DEFINITION_SHAPE ( 'NONE', 'NONE',  #2485 ) ;
#6044 = ADVANCED_FACE ( 'NONE', ( #2044 ), #10323, .T. ) ;
#6045 = CARTESIAN_POINT ( 'NONE',  ( 8.526344538924147898, 0.8706977022493568308, 0.3793004607997266797 ) ) ;
#6046 = DIRECTION ( 'NONE',  ( 0.4999999999999998890, 0.000000000000000000, -0.8660254037844385966 ) ) ;
#6047 = VECTOR ( 'NONE', #8922, 39.37007874015748143 ) ;
#6048 = DIRECTION ( 'NONE',  ( 0.000000000000000000, 0.000000000000000000, -1.000000000000000000 ) ) ;
#6049 = CARTESIAN_POINT ( 'NONE',  ( 4.040612674447555897, 1.739716132213777522, 0.7790939297231012084 ) ) ;
#6050 = EDGE_LOOP ( 'NONE', ( #12517, #14003, #7015, #6285 ) ) ;
#6051 = DIRECTION ( 'NONE',  ( 0.000000000000000000, 0.000000000000000000, -1.000000000000000000 ) ) ;
#6053 = VERTEX_POINT ( 'NONE', #9180 ) ;
#6052 = FACE_OUTER_BOUND ( 'NONE', #5252, .T. ) ;
#6054 = ORIENTED_EDGE ( 'NONE', *, *, #14737, .T. ) ;
#6055 = AXIS2_PLACEMENT_3D ( 'NONE', #13973, #7044, #4738 ) ;
#6056 = FACE_OUTER_BOUND ( 'NONE', #13218, .T. ) ;
#6057 = CARTESIAN_POINT ( 'NONE',  ( 2.855088541747415221, 0.5369222675350757701, 0.4596738906534074132 ) ) ;
#6058 = VERTEX_POINT ( 'NONE', #13905 ) ;
#6059 = DIRECTION ( 'NONE',  ( -0.000000000000000000, -1.000000000000000000, -0.000000000000000000 ) ) ;
#6060 = CIRCLE ( 'NONE', #12670, 2.500000000000000000 ) ;
#6061 = FACE_BOUND ( 'NONE', #13069, .T. ) ;
#6062 = EDGE_CURVE ( 'NONE', #13231, #9310, #5590, .T. ) ;
#6063 = CARTESIAN_POINT ( 'NONE',  ( 9.797174393178826150E-17, 0.1749999999999999889, 0.8000000000000000444 ) ) ;
#6064 = CIRCLE ( 'NONE', #12166, 0.06000000000000001166 ) ;
#6065 = ADVANCED_FACE ( 'NONE', ( #14986 ), #13257, .F. ) ;
#6066 = ORIENTED_EDGE ( 'NONE', *, *, #13005, .F. ) ;
#6067 = CARTESIAN_POINT ( 'NONE',  ( 3.426491571325181340, 1.679378605318059048, 1.679378605318041506 ) ) ;
#6068 = EDGE_CURVE ( 'NONE', #5706, #12243, #11547, .T. ) ;
#6069 = CARTESIAN_POINT ( 'NONE',  ( 0.6766392826275051675, -0.4261666590922867370, 0.4729147972023082236 ) ) ;
#6070 = CARTESIAN_POINT ( 'NONE',  ( 3.874999999999999556, 3.105999999999998984, 1.130000000000000560 ) ) ;
#6071 = DIRECTION ( 'NONE',  ( -1.000000000000000000, -0.000000000000000000, -0.000000000000000000 ) ) ;
#6072 = ORIENTED_EDGE ( 'NONE', *, *, #1676, .F. ) ;
#6073 = AXIS2_PLACEMENT_3D ( 'NONE', #5789, #3651, #11599 ) ;
#6074 = CARTESIAN_POINT ( 'NONE',  ( 3.426491571325181340, -0.6999999999999989564, -2.399999999999999911 ) ) ;
#6075 = ORIENTED_EDGE ( 'NONE', *, *, #2600, .T. ) ;
#6076 = EDGE_CURVE ( 'NONE', #2531, #2396, #7047, .T. ) ;
#6077 = DIRECTION ( 'NONE',  ( 0.000000000000000000, 0.000000000000000000, -1.000000000000000000 ) ) ;
#6078 = APPLICATION_CONTEXT ( 'automotive_design' ) ;
#6079 = EDGE_LOOP ( 'NONE', ( #10369, #3375 ) ) ;
#6080 = EDGE_CURVE ( 'NONE', #801, #9252, #2026, .T. ) ;
#6081 = CARTESIAN_POINT ( 'NONE',  ( 6.826491571325181695, 1.679378605318035733, -2.054378605318066153 ) ) ;
#6082 = CARTESIAN_POINT ( 'NONE',  ( 0.000000000000000000, 1.503199999999999870, 0.000000000000000000 ) ) ;
#6083 = VECTOR ( 'NONE', #10409, 39.37007874015748143 ) ;
#6084 = DIRECTION ( 'NONE',  ( -0.000000000000000000, 1.000000000000000000, -0.000000000000000000 ) ) ;
#6085 = VECTOR ( 'NONE', #8549, 39.37007874015748143 ) ;
#6086 = CARTESIAN_POINT ( 'NONE',  ( 2.774999999999999911, 0.9799999999999438050, -2.360000000000016307 ) ) ;
#6087 = CIRCLE ( 'NONE', #10959, 0.4070000000000044138 ) ;
#6088 = FACE_OUTER_BOUND ( 'NONE', #12976, .T. ) ;
#6089 = VECTOR ( 'NONE', #9730, 39.37007874015748854 ) ;
#6090 = VERTEX_POINT ( 'NONE', #1209 ) ;
#6091 = VERTEX_POINT ( 'NONE', #4742 ) ;
#6092 = AXIS2_PLACEMENT_3D ( 'NONE', #10803, #4924, #8443 ) ;
#6093 = ORIENTED_EDGE ( 'NONE', *, *, #14636, .T. ) ;
#6094 = EDGE_CURVE ( 'NONE', #3613, #4636, #3264, .T. ) ;
#6095 = CARTESIAN_POINT ( 'NONE',  ( 1.004574810408579433, -0.4429999999999998384, -0.3264278243218214359 ) ) ;
#6096 = AXIS2_PLACEMENT_3D ( 'NONE', #5001, #11095, #2701 ) ;
#6097 = LINE ( 'NONE', #13108, #8194 ) ;
#6098 = EDGE_CURVE ( 'NONE', #9866, #13738, #11625, .T. ) ;
#6099 = CARTESIAN_POINT ( 'NONE',  ( 2.061999999999999833, 0.000000000000000000, 0.000000000000000000 ) ) ;
#6100 = AXIS2_PLACEMENT_3D ( 'NONE', #3119, #8854, #13345 ) ;
#6101 = CARTESIAN_POINT ( 'NONE',  ( 3.394491571325183088, -1.679378605318041950, 1.416878605318058870 ) ) ;
#6102 = ORIENTED_EDGE ( 'NONE', *, *, #5881, .T. ) ;
#6103 = VECTOR ( 'NONE', #14420, 39.37007874015748143 ) ;
#6104 = DIRECTION ( 'NONE',  ( 0.000000000000000000, 0.000000000000000000, -1.000000000000000000 ) ) ;
#6105 = ADVANCED_FACE ( 'NONE', ( #9340 ), #13977, .T. ) ;
#6106 = CARTESIAN_POINT ( 'NONE',  ( 1.814459835756555783, 0.1490781312163585171, 0.4743720362179413286 ) ) ;
#6107 = FILL_AREA_STYLE_COLOUR ( '', #13691 ) ;
#6108 = CARTESIAN_POINT ( 'NONE',  ( 2.124999999999999556, 1.574999999999994849, -1.575000000000022160 ) ) ;
#6109 = AXIS2_PLACEMENT_3D ( 'NONE', #2725, #14563, #8838 ) ;
#6110 = CARTESIAN_POINT ( 'NONE',  ( 4.263277331923934099, 1.731577658895514071, -0.6428753901762764844 ) ) ;
#6111 = ORIENTED_EDGE ( 'NONE', *, *, #2010, .F. ) ;
#6113 = VERTEX_POINT ( 'NONE', #12836 ) ;
#6112 = CARTESIAN_POINT ( 'NONE',  ( 0.7007556580885034858, -0.4010748535711006202, -0.4875099722676211056 ) ) ;
#6114 = EDGE_LOOP ( 'NONE', ( #9028, #8404, #4582, #4918, #7456 ) ) ;
#6115 = CARTESIAN_POINT ( 'NONE',  ( 3.874999999999999556, 3.137999999999999901, -1.542000000000000037 ) ) ;
#6116 = EDGE_LOOP ( 'NONE', ( #11341, #11837, #3276, #8147 ) ) ;
#6117 = DIRECTION ( 'NONE',  ( -0.000000000000000000, -1.000000000000000000, -0.000000000000000000 ) ) ;
#6118 = DIRECTION ( 'NONE',  ( 0.9994964035307943861, 0.000000000000000000, 0.03173230733822608035 ) ) ;
#6119 = CYLINDRICAL_SURFACE ( 'NONE', #12570, 0.9499999999999988454 ) ;
#6120 = ORIENTED_EDGE ( 'NONE', *, *, #3705, .F. ) ;
#6121 = CARTESIAN_POINT ( 'NONE',  ( 2.742999999999998995, -1.679378605318059048, -1.941878605318027251 ) ) ;
#6122 = LINE ( 'NONE', #1205, #14143 ) ;
#6123 = AXIS2_PLACEMENT_3D ( 'NONE', #14055, #9264, #8041 ) ;
#6124 = EDGE_CURVE ( 'NONE', #626, #6575, #14668, .T. ) ;
#6125 = DIRECTION ( 'NONE',  ( -0.000000000000000000, -1.000000000000000000, -0.000000000000000000 ) ) ;
#6126 = CARTESIAN_POINT ( 'NONE',  ( 3.874999999999999556, 3.137999999999999901, 1.320000000000000062 ) ) ;
#6127 = CARTESIAN_POINT ( 'NONE',  ( 2.061999999999999389, 0.000000000000000000, -1.409999999999999920 ) ) ;
#6128 = CARTESIAN_POINT ( 'NONE',  ( 0.8232171895119964056, -0.4398285061085906444, -0.4481849241520746152 ) ) ;
#6129 = CARTESIAN_POINT ( 'NONE',  ( 3.643781337222963046, 1.948212547232942127, 0.7131559760554623262 ) ) ;
#6130 = DIRECTION ( 'NONE',  ( -5.329070518200750763E-14, 0.000000000000000000, -1.000000000000000000 ) ) ;
#6131 = VERTEX_POINT ( 'NONE', #2369 ) ;
#6132 = CARTESIAN_POINT ( 'NONE',  ( 0.6733268703976357239, -0.4720969008048874760, 0.4545075337565439577 ) ) ;
#6134 = ORIENTED_EDGE ( 'NONE', *, *, #3705, .T. ) ;
#6133 = CARTESIAN_POINT ( 'NONE',  ( 0.000000000000000000, 0.000000000000000000, 0.000000000000000000 ) ) ;
#6135 = EDGE_LOOP ( 'NONE', ( #14555, #2685 ) ) ;
#6136 = CARTESIAN_POINT ( 'NONE',  ( 3.426491571325181340, 1.679378605318059048, 1.384878605318043521 ) ) ;
#6137 = ORIENTED_EDGE ( 'NONE', *, *, #1226, .T. ) ;
#6138 = DIRECTION ( 'NONE',  ( -1.000000000000000000, -0.000000000000000000, -0.000000000000000000 ) ) ;
#6139 = VECTOR ( 'NONE', #12665, 39.37007874015748854 ) ;
#6140 = EDGE_CURVE ( 'NONE', #14179, #6889, #8638, .T. ) ;
#6141 = DIRECTION ( 'NONE',  ( 1.000000000000000000, 0.000000000000000000, 0.000000000000000000 ) ) ;
#6142 = LINE ( 'NONE', #5143, #8530 ) ;
#6143 = ORIENTED_EDGE ( 'NONE', *, *, #9449, .T. ) ;
#6144 = DIRECTION ( 'NONE',  ( -0.000000000000000000, -1.000000000000000000, -0.000000000000000000 ) ) ;
#6145 = DIRECTION ( 'NONE',  ( 0.000000000000000000, 0.000000000000000000, 1.000000000000000000 ) ) ;
#6146 = CARTESIAN_POINT ( 'NONE',  ( 2.774999999999999911, 1.575000000000000178, -2.360000000000016751 ) ) ;
#6147 = EDGE_LOOP ( 'NONE', ( #9432, #8795, #7083 ) ) ;
#6148 = CARTESIAN_POINT ( 'NONE',  ( 0.2372115730956756152, 0.1749999999999999889, -0.8852856429364902580 ) ) ;
#6149 = DIRECTION ( 'NONE',  ( 0.000000000000000000, 0.000000000000000000, -1.000000000000000000 ) ) ;
#6150 = EDGE_LOOP ( 'NONE', ( #8089, #1660, #2800, #4482 ) ) ;
#6151 = CARTESIAN_POINT ( 'NONE',  ( -0.2936244729112616469, 1.600827805288695949, 0.2533330005240802540 ) ) ;
#6152 = ORIENTED_EDGE ( 'NONE', *, *, #13329, .T. ) ;
#6153 = EDGE_CURVE ( 'NONE', #4391, #14462, #9381, .T. ) ;
#6154 = EDGE_CURVE ( 'NONE', #2972, #11468, #3822, .T. ) ;
#6155 = ADVANCED_FACE ( 'NONE', ( #3598 ), #2674, .F. ) ;
#6156 = CARTESIAN_POINT ( 'NONE',  ( 3.875000000000000000, 0.7099999999999984102, -0.4849999999999995981 ) ) ;
#6157 = DIRECTION ( 'NONE',  ( -1.000000000000000000, 0.000000000000000000, 0.000000000000000000 ) ) ;
#6158=STYLED_ITEM('',(#15206),#5275);
#6159 = CARTESIAN_POINT ( 'NONE',  ( 0.09500000000000431710, 1.679378605318059492, 2.054378605318042172 ) ) ;
#6160 = EDGE_CURVE ( 'NONE', #11668, #4452, #14250, .T. ) ;
#6161 = CARTESIAN_POINT ( 'NONE',  ( 3.426491571325181340, 0.000000000000000000, 2.500000000000000444 ) ) ;
#6162 = ORIENTED_EDGE ( 'NONE', *, *, #9430, .F. ) ;
#6163 = EDGE_LOOP ( 'NONE', ( #10676, #11733, #4963, #6262 ) ) ;
#6164 = ORIENTED_EDGE ( 'NONE', *, *, #7176, .F. ) ;
#6165 = CARTESIAN_POINT ( 'NONE',  ( 8.526344538923749994, 0.8706977022493430640, -0.3793004607997343958 ) ) ;
#6166 =( GEOMETRIC_REPRESENTATION_CONTEXT ( 3 ) GLOBAL_UNCERTAINTY_ASSIGNED_CONTEXT ( ( #10145 ) ) GLOBAL_UNIT_ASSIGNED_CONTEXT ( ( #4491, #11528, #5566 ) ) REPRESENTATION_CONTEXT ( 'NONE', 'WORKASPACE' ) );
#6167 = CARTESIAN_POINT ( 'NONE',  ( 0.8108060929038570785, -0.4429999999999998939, -0.3024090436974096185 ) ) ;
#6168 = DIRECTION ( 'NONE',  ( -1.000000000000000000, 0.000000000000000000, -1.047444401652940007E-14 ) ) ;
#6169 = CARTESIAN_POINT ( 'NONE',  ( 2.001999999999999780, 0.000000000000000000, 0.000000000000000000 ) ) ;
#6170 = CYLINDRICAL_SURFACE ( 'NONE', #1687, 0.5000000000000002220 ) ;
#6171 = LINE ( 'NONE', #10831, #8773 ) ;
#6172 = DIRECTION ( 'NONE',  ( 1.000000000000000000, 0.000000000000000000, 0.000000000000000000 ) ) ;
#6173 = AXIS2_PLACEMENT_3D ( 'NONE', #7899, #12549, #13848 ) ;
#6174 = CARTESIAN_POINT ( 'NONE',  ( -0.7287617923574205570, 0.2159999999999999420, 0.4425000000000005596 ) ) ;
#6175 = EDGE_CURVE ( 'NONE', #159, #3499, #11851, .T. ) ;
#6176 = ORIENTED_EDGE ( 'NONE', *, *, #8011, .T. ) ;
#6177 = CONICAL_SURFACE ( 'NONE', #5937, 0.2625000000000000111, 0.7853981633974503884 ) ;
#6179 = VERTEX_POINT ( 'NONE', #11781 ) ;
#6178 = CARTESIAN_POINT ( 'NONE',  ( 0.7006934119264053296, -0.4055938261068608996, -0.4858827016952778632 ) ) ;
#6180 = ADVANCED_FACE ( 'NONE', ( #9569 ), #2598, .F. ) ;
#6181 = EDGE_LOOP ( 'NONE', ( #15013, #3814 ) ) ;
#6182 = CARTESIAN_POINT ( 'NONE',  ( 0.07252880680210851971, 1.600831684639946850, 0.3809527529760087239 ) ) ;
#6183 = CIRCLE ( 'NONE', #527, 0.1000000000000000194 ) ;
#6184 = DIRECTION ( 'NONE',  ( 0.000000000000000000, 0.000000000000000000, -1.000000000000000000 ) ) ;
#6185 = PRODUCT_CONTEXT ( 'NONE', #2936, 'mechanical' ) ;
#6186 = FACE_OUTER_BOUND ( 'NONE', #8244, .T. ) ;
#6187 = ORIENTED_EDGE ( 'NONE', *, *, #3326, .T. ) ;
#6188 = CARTESIAN_POINT ( 'NONE',  ( -0.4125000000000001998, 0.2159999999999999698, -0.3725000000000000533 ) ) ;
#6189 = DIRECTION ( 'NONE',  ( 0.000000000000000000, 0.000000000000000000, -1.000000000000000000 ) ) ;
#6190 = CARTESIAN_POINT ( 'NONE',  ( 3.874999999999999556, 3.105999999999998984, -1.509999999999999787 ) ) ;
#6191 = CARTESIAN_POINT ( 'NONE',  ( 0.1164708448095412852, 0.1749999999999999889, -0.9176380235743023528 ) ) ;
#6192 = FACE_OUTER_BOUND ( 'NONE', #5856, .T. ) ;
#6193 = CARTESIAN_POINT ( 'NONE',  ( 0.8575369771065451951, -0.4333177464522090516, -0.4606414905107603652 ) ) ;
#6195 = ORIENTED_EDGE ( 'NONE', *, *, #11829, .F. ) ;
#6194 = CARTESIAN_POINT ( 'NONE',  ( 6.176491571325181340, 0.000000000000000000, 0.000000000000000000 ) ) ;
#6196 = EDGE_CURVE ( 'NONE', #3491, #12114, #3022, .T. ) ;
#6197 = EDGE_CURVE ( 'NONE', #5661, #1040, #5475, .T. ) ;
#6198 = ORIENTED_EDGE ( 'NONE', *, *, #12596, .F. ) ;
#6199 = AXIS2_PLACEMENT_3D ( 'NONE', #1115, #12672, #8342 ) ;
#6200 = DIRECTION ( 'NONE',  ( 0.7071067811865519026, 8.659560562354877391E-17, 0.7071067811865430208 ) ) ;
#6202 = ORIENTED_EDGE ( 'NONE', *, *, #8982, .T. ) ;
#6201 = FACE_OUTER_BOUND ( 'NONE', #7797, .T. ) ;
#6203 = VERTEX_POINT ( 'NONE', #1917 ) ;
#6204 = TOROIDAL_SURFACE ( 'NONE', #14741, 0.1150000000000000050, 0.04000000000000000083 ) ;
#6205 = DIRECTION ( 'NONE',  ( 1.655665450705613915E-16, 3.103226861728128995E-32, 1.000000000000000000 ) ) ;
#6206 = LENGTH_MEASURE_WITH_UNIT ( LENGTH_MEASURE( 0.02539999999999999897 ), #6361 );
#6207 = CARTESIAN_POINT ( 'NONE',  ( 2.774999999999999911, 1.575000000000016609, 1.575000000000000178 ) ) ;
#6208 = ORIENTED_EDGE ( 'NONE', *, *, #12366, .F. ) ;
#6209 = AXIS2_PLACEMENT_3D ( 'NONE', #3517, #7959, #14061 ) ;
#6210 = DIRECTION ( 'NONE',  ( 0.000000000000000000, 0.000000000000000000, -1.000000000000000000 ) ) ;
#6211 = CARTESIAN_POINT ( 'NONE',  ( 0.6782188896242594689, -0.01324371508926007121, 0.4691064452754763470 ) ) ;
#6212 = AXIS2_PLACEMENT_3D ( 'NONE', #6067, #4408, #6859 ) ;
#6213 = DIRECTION ( 'NONE',  ( 0.000000000000000000, 0.000000000000000000, -1.000000000000000000 ) ) ;
#6214 = ORIENTED_EDGE ( 'NONE', *, *, #11883, .F. ) ;
#6215 = DIRECTION ( 'NONE',  ( 0.000000000000000000, 0.000000000000000000, -1.000000000000000000 ) ) ;
#6216 = CARTESIAN_POINT ( 'NONE',  ( 0.000000000000000000, 1.000000000000000000, -0.6614378277661475680 ) ) ;
#6217 = CARTESIAN_POINT ( 'NONE',  ( 2.775039370078740131, -1.679378605318047946, -1.679378605318053497 ) ) ;
#6218 = EDGE_LOOP ( 'NONE', ( #14232, #13319, #8315, #11539 ) ) ;
#6219 = DIRECTION ( 'NONE',  ( 0.000000000000000000, 0.000000000000000000, 1.000000000000000000 ) ) ;
#6220 = ORIENTED_EDGE ( 'NONE', *, *, #5349, .T. ) ;
#6221 = CARTESIAN_POINT ( 'NONE',  ( 0.7238317330277964645, -0.005069019069653440263, 0.4548041668469371412 ) ) ;
#6222 = VERTEX_POINT ( 'NONE', #1760 ) ;
#6223 = AXIS2_PLACEMENT_3D ( 'NONE', #10788, #350, #1727 ) ;
#6224 = DIRECTION ( 'NONE',  ( 0.000000000000000000, 0.000000000000000000, -1.000000000000000000 ) ) ;
#6225 = DIRECTION ( 'NONE',  ( -0.000000000000000000, -1.000000000000000000, -0.000000000000000000 ) ) ;
#6226 = CARTESIAN_POINT ( 'NONE',  ( 0.8254245316410399047, -0.4429999999999996163, -0.3670313414528083573 ) ) ;
#6227 = DIRECTION ( 'NONE',  ( -1.000000000000000000, -0.000000000000000000, -0.000000000000000000 ) ) ;
#6228 = CIRCLE ( 'NONE', #5996, 1.932031071636253650 ) ;
#6229 = CARTESIAN_POINT ( 'NONE',  ( 2.774999999999999911, 2.360000000000015863, 1.574999999999999956 ) ) ;
#6230 = ADVANCED_FACE ( 'NONE', ( #4231 ), #2166, .T. ) ;
#6231 = VECTOR ( 'NONE', #12109, 39.37007874015748143 ) ;
#6232 = VECTOR ( 'NONE', #8807, 39.37007874015748854 ) ;
#6233 = EDGE_CURVE ( 'NONE', #12635, #13163, #5221, .T. ) ;
#6234 = ORIENTED_EDGE ( 'NONE', *, *, #14133, .T. ) ;
#6235 = VERTEX_POINT ( 'NONE', #5611 ) ;
#6236 = VERTEX_POINT ( 'NONE', #10421 ) ;
#6237 = DIRECTION ( 'NONE',  ( 0.000000000000000000, 0.000000000000000000, 1.000000000000000000 ) ) ;
#6238 = DIRECTION ( 'NONE',  ( -0.000000000000000000, 1.000000000000000000, -0.000000000000000000 ) ) ;
#6239 = CARTESIAN_POINT ( 'NONE',  ( 4.769268701363833074, 3.137999999999999901, -0.3249191361593796734 ) ) ;
#6240 = EDGE_CURVE ( 'NONE', #331, #14332, #10272, .T. ) ;
#6241 = CIRCLE ( 'NONE', #7951, 0.2944999999999998175 ) ;
#6242 = DIRECTION ( 'NONE',  ( 0.000000000000000000, 0.000000000000000000, -1.000000000000000000 ) ) ;
#6243 = DIRECTION ( 'NONE',  ( 0.000000000000000000, 0.000000000000000000, 1.000000000000000000 ) ) ;
#6244 = VECTOR ( 'NONE', #5507, 39.37007874015748143 ) ;
#6245 = AXIS2_PLACEMENT_3D ( 'NONE', #2377, #11721, #13755 ) ;
#6246 = CARTESIAN_POINT ( 'NONE',  ( 4.621667715411809318, 1.809504207475592485, 0.09880105512956799396 ) ) ;
#6247 = DIRECTION ( 'NONE',  ( 0.000000000000000000, 0.000000000000000000, 1.000000000000000000 ) ) ;
#6248 = EDGE_CURVE ( 'NONE', #7097, #14200, #3304, .T. ) ;
#6249 = AXIS2_PLACEMENT_3D ( 'NONE', #8735, #13230, #14396 ) ;
#6250 = ADVANCED_FACE ( 'NONE', ( #10439 ), #13751, .T. ) ;
#6251 = VERTEX_POINT ( 'NONE', #6127 ) ;
#6252 = AXIS2_PLACEMENT_3D ( 'NONE', #5820, #10485, #12606 ) ;
#6253 = ORIENTED_EDGE ( 'NONE', *, *, #12679, .T. ) ;
#6254 = AXIS2_PLACEMENT_3D ( 'NONE', #15032, #5638, #10221 ) ;
#6255 = VERTEX_POINT ( 'NONE', #10785 ) ;
#6256 = DIRECTION ( 'NONE',  ( 0.000000000000000000, 0.000000000000000000, -1.000000000000000000 ) ) ;
#6257 = CARTESIAN_POINT ( 'NONE',  ( 0.2499999999999999722, 0.000000000000000000, 0.000000000000000000 ) ) ;
#6258 = DIRECTION ( 'NONE',  ( -1.000000000000000000, -0.000000000000000000, -0.000000000000000000 ) ) ;
#6259 = EDGE_CURVE ( 'NONE', #9681, #6058, #2540, .T. ) ;
#6260 = APPLICATION_PROTOCOL_DEFINITION ( 'draft international standard', 'automotive_design', 1998, #1558 ) ;
#6261 = CARTESIAN_POINT ( 'NONE',  ( 2.715751415184836315, 0.8549853309850858896, 0.4616419291641825073 ) ) ;
#6262 = ORIENTED_EDGE ( 'NONE', *, *, #7382, .F. ) ;
#6263 = CARTESIAN_POINT ( 'NONE',  ( 6.794491571325181667, 1.679378605318059492, 1.304378605318041062 ) ) ;
#6264 = DIRECTION ( 'NONE',  ( 0.000000000000000000, 0.000000000000000000, -1.000000000000000000 ) ) ;
#6265 = ADVANCED_FACE ( 'NONE', ( #13277 ), #6447, .T. ) ;
#6266 = CIRCLE ( 'NONE', #6500, 0.4849999999999995981 ) ;
#6267 = CARTESIAN_POINT ( 'NONE',  ( 3.458515826269089377, 2.043633784419520705, 0.6239720965697329591 ) ) ;
#6268 = AXIS2_PLACEMENT_3D ( 'NONE', #2329, #8240, #7164 ) ;
#6269 = VECTOR ( 'NONE', #1999, 39.37007874015748143 ) ;
#6270 = ADVANCED_FACE ( 'NONE', ( #2028 ), #11553, .T. ) ;
#6271 = CARTESIAN_POINT ( 'NONE',  ( 0.8336852985356731915, -0.4829999999999998739, -0.4100337033397443709 ) ) ;
#6272 = LINE ( 'NONE', #9713, #4716 ) ;
#6273 = CARTESIAN_POINT ( 'NONE',  ( 3.807348201284447953, 1.879736805572670422, 0.7469949793200116872 ) ) ;
#6274 = CARTESIAN_POINT ( 'NONE',  ( 3.874999999999999556, 3.105999999999998984, -1.509999999999999787 ) ) ;
#6275 = AXIS2_PLACEMENT_3D ( 'NONE', #14677, #13669, #10094 ) ;
#6276 = ORIENTED_EDGE ( 'NONE', *, *, #364, .F. ) ;
#6277 = CARTESIAN_POINT ( 'NONE',  ( 1.000000000000000222, -0.4829999999999998739, -0.3182109165419976238 ) ) ;
#6279 = ORIENTED_EDGE ( 'NONE', *, *, #6154, .T. ) ;
#6278 = FACE_OUTER_BOUND ( 'NONE', #5192, .T. ) ;
#6280 = VERTEX_POINT ( 'NONE', #3142 ) ;
#6281 = ADVANCED_FACE ( 'NONE', ( #2211 ), #11073, .F. ) ;
#6282 = DIRECTION ( 'NONE',  ( 0.000000000000000000, 1.000000000000000000, 0.000000000000000000 ) ) ;
#6283 =( LENGTH_UNIT ( ) NAMED_UNIT ( * ) SI_UNIT ( $, .METRE. ) );
#6284 = CYLINDRICAL_SURFACE ( 'NONE', #12084, 0.4849999999999995981 ) ;
#6285 = ORIENTED_EDGE ( 'NONE', *, *, #10442, .F. ) ;
#6286 = CARTESIAN_POINT ( 'NONE',  ( 0.8999999999999999112, -0.6230000000000016636, -0.4500000000000000666 ) ) ;
#6287 = DIMENSIONAL_EXPONENTS ( 1.000000000000000000, 0.000000000000000000, 0.000000000000000000, 0.000000000000000000, 0.000000000000000000, 0.000000000000000000, 0.000000000000000000 ) ;
#6288 = EDGE_CURVE ( 'NONE', #7285, #3185, #8414, .T. ) ;
#6289 = VECTOR ( 'NONE', #3027, 39.37007874015748143 ) ;
#6290 = CARTESIAN_POINT ( 'NONE',  ( 0.7117500205948168457, -0.01337125625712030051, 0.4679153652930429508 ) ) ;
#6291 = DIRECTION ( 'NONE',  ( 1.000000000000000000, 0.000000000000000000, 0.000000000000000000 ) ) ;
#6292 = ORIENTED_EDGE ( 'NONE', *, *, #3534, .T. ) ;
#6293 = DIRECTION ( 'NONE',  ( -0.7071067811865479058, 8.659560562354927928E-17, -0.7071067811865471286 ) ) ;
#6294 = CIRCLE ( 'NONE', #14830, 0.8499999999999999778 ) ;
#6295 = CARTESIAN_POINT ( 'NONE',  ( -0.4425000000000007261, 0.2159999999999999420, -0.8499999999999999778 ) ) ;
#6296 = CARTESIAN_POINT ( 'NONE',  ( 0.000000000000000000, 1.812500000000000222, 0.000000000000000000 ) ) ;
#6297 = CYLINDRICAL_SURFACE ( 'NONE', #6249, 0.1899999999999996136 ) ;
#6298 = ORIENTED_EDGE ( 'NONE', *, *, #9053, .F. ) ;
#6299 = SPHERICAL_SURFACE ( 'NONE', #9140, 1.000000000000000000 ) ;
#6300 = ORIENTED_EDGE ( 'NONE', *, *, #7927, .T. ) ;
#6301 = CARTESIAN_POINT ( 'NONE',  ( 3.426491571325181340, -1.574999999999984190, 1.575000000000033040 ) ) ;
#6302 = CARTESIAN_POINT ( 'NONE',  ( 0.3724999999999999423, 0.2159999999999999698, 0.3724999999999999423 ) ) ;
#6303 = EDGE_CURVE ( 'NONE', #5917, #2036, #3441, .T. ) ;
#6304 = DIRECTION ( 'NONE',  ( 1.000000000000000000, 0.000000000000000000, 0.000000000000000000 ) ) ;
#6305 = LINE ( 'NONE', #8744, #183 ) ;
#6306 = CARTESIAN_POINT ( 'NONE',  ( 6.176491571325181340, 1.679378605318035733, -2.086378605318067958 ) ) ;
#6307 = CARTESIAN_POINT ( 'NONE',  ( 6.176491571325181340, 1.679378605318059492, 2.086378605318043533 ) ) ;
#6308 = CIRCLE ( 'NONE', #9969, 0.3203340137431719414 ) ;
#6309 = ORIENTED_EDGE ( 'NONE', *, *, #2588, .T. ) ;
#6310 = ORIENTED_EDGE ( 'NONE', *, *, #13754, .T. ) ;
#6311 = AXIS2_PLACEMENT_3D ( 'NONE', #12933, #2382, #9506 ) ;
#6312 = ORIENTED_EDGE ( 'NONE', *, *, #7399, .T. ) ;
#6313 = DIRECTION ( 'NONE',  ( -1.000000000000000000, -0.000000000000000000, -0.000000000000000000 ) ) ;
#6314 = DIRECTION ( 'NONE',  ( 1.000000000000000000, 0.000000000000000000, 0.000000000000000000 ) ) ;
#6315 = AXIS2_PLACEMENT_3D ( 'NONE', #4218, #3292, #5285 ) ;
#6316 = DIRECTION ( 'NONE',  ( -0.000000000000000000, -1.000000000000000000, -0.000000000000000000 ) ) ;
#6317 = FACE_OUTER_BOUND ( 'NONE', #5005, .T. ) ;
#6318 = AXIS2_PLACEMENT_3D ( 'NONE', #8333, #2569, #12965 ) ;
#6319 = CARTESIAN_POINT ( 'NONE',  ( 3.426491571325181784, 2.056034060376116024, -0.5999481385559809477 ) ) ;
#6320 = AXIS2_PLACEMENT_3D ( 'NONE', #8511, #1296, #13220 ) ;
#6321 = CARTESIAN_POINT ( 'NONE',  ( 4.607097790994713726, 1.806582460388006073, 0.1715432876979409993 ) ) ;
#6322 = PRODUCT_DEFINITION ( 'UNKNOWN', '', #11587, #12275 ) ;
#6323 = CARTESIAN_POINT ( 'NONE',  ( 0.4124999999999997558, 0.1859999999999983611, -0.4125000000000000333 ) ) ;
#6324 = VECTOR ( 'NONE', #3460, 39.37007874015748143 ) ;
#6325 = VECTOR ( 'NONE', #1657, 39.37007874015748854 ) ;
#6326 = CIRCLE ( 'NONE', #11439, 1.000000000000000444 ) ;
#6327 = AXIS2_PLACEMENT_3D ( 'NONE', #10509, #9595, #2547 ) ;
#6328 = CARTESIAN_POINT ( 'NONE',  ( 4.264972657050305038, 1.781419589088464317, -0.6418377093470817307 ) ) ;
#6329 = ORIENTED_EDGE ( 'NONE', *, *, #5430, .F. ) ;
#6330 = ORIENTED_EDGE ( 'NONE', *, *, #822, .F. ) ;
#6331 = AXIS2_PLACEMENT_3D ( 'NONE', #6040, #1350, #11778 ) ;
#6332 = VECTOR ( 'NONE', #8931, 39.37007874015748143 ) ;
#6333 = ORIENTED_EDGE ( 'NONE', *, *, #4896, .F. ) ;
#6334 = CARTESIAN_POINT ( 'NONE',  ( 3.394491571325183088, -1.679378605318041950, 1.679378605318059048 ) ) ;
#6335 = CARTESIAN_POINT ( 'NONE',  ( 0.000000000000000000, 1.629999999999999893, 0.000000000000000000 ) ) ;
#6336 = PLANE ( 'NONE',  #13295 ) ;
#6337 = DIRECTION ( 'NONE',  ( -0.000000000000000000, -1.000000000000000000, -0.000000000000000000 ) ) ;
#6338 = ORIENTED_EDGE ( 'NONE', *, *, #10260, .F. ) ;
#6339 = DIRECTION ( 'NONE',  ( 1.000000000000000000, 0.000000000000000000, 0.000000000000000000 ) ) ;
#6340 = CARTESIAN_POINT ( 'NONE',  ( 4.769268701363833074, 3.137999999999999901, 0.3249191361593796734 ) ) ;
#6341 = ADVANCED_FACE ( 'NONE', ( #2128 ), #7430, .F. ) ;
#6342 = EDGE_CURVE ( 'NONE', #12132, #9031, #14834, .T. ) ;
#6343 = LINE ( 'NONE', #8702, #12920 ) ;
#6344 = EDGE_CURVE ( 'NONE', #4913, #2874, #4363, .T. ) ;
#6345=STYLED_ITEM('',(#15171),#10609);
#6346 = AXIS2_PLACEMENT_3D ( 'NONE', #10605, #14191, #6104 ) ;
#6347 = FACE_OUTER_BOUND ( 'NONE', #2543, .T. ) ;
#6348 = EDGE_CURVE ( 'NONE', #11724, #733, #10180, .T. ) ;
#6349 = CARTESIAN_POINT ( 'NONE',  ( 0.8336852985356729695, -0.4430000000000001714, -0.4100337033397444264 ) ) ;
#6350 = ADVANCED_FACE ( 'NONE', ( #13678 ), #13036, .F. ) ;
#6351 = LINE ( 'NONE', #11002, #5356 ) ;
#6353 = ORIENTED_EDGE ( 'NONE', *, *, #4290, .T. ) ;
#6352 = FACE_OUTER_BOUND ( 'NONE', #6648, .T. ) ;
#6354 = ORIENTED_EDGE ( 'NONE', *, *, #14567, .T. ) ;
#6355 = DIRECTION ( 'NONE',  ( 1.000000000000000000, -2.602462600580851747E-17, 0.000000000000000000 ) ) ;
#6357 = ORIENTED_EDGE ( 'NONE', *, *, #4972, .T. ) ;
#6356 = FACE_BOUND ( 'NONE', #4811, .T. ) ;
#6358 = ORIENTED_EDGE ( 'NONE', *, *, #14263, .F. ) ;
#6359 = CIRCLE ( 'NONE', #14404, 2.070731779878276502 ) ;
#6360 = CARTESIAN_POINT ( 'NONE',  ( 2.187203820042824542, 0.4712135623730921985, -0.4085020630706684974 ) ) ;
#6361 =( LENGTH_UNIT ( ) NAMED_UNIT ( * ) SI_UNIT ( $, .METRE. ) );
#6362 = DIRECTION ( 'NONE',  ( 0.000000000000000000, 0.000000000000000000, -1.000000000000000000 ) ) ;
#6363 = VERTEX_POINT ( 'NONE', #6817 ) ;
#6364 = DIRECTION ( 'NONE',  ( 1.000000000000000000, 0.000000000000000000, 0.000000000000000000 ) ) ;
#6365 = DIRECTION ( 'NONE',  ( 0.000000000000000000, 1.000000000000000000, 0.000000000000000000 ) ) ;
#6366 = CARTESIAN_POINT ( 'NONE',  ( 0.7241094260644624914, -0.005263640177536527999, 0.4546250289485997964 ) ) ;
#6367 = LINE ( 'NONE', #14308, #9260 ) ;
#6368 = EDGE_LOOP ( 'NONE', ( #8865, #1549 ) ) ;
#6369 = CARTESIAN_POINT ( 'NONE',  ( 0.6601485485260571995, -0.07064835164835162051, -0.5137583810202324131 ) ) ;
#6370 = FACE_OUTER_BOUND ( 'NONE', #3587, .T. ) ;
#6371 = SURFACE_STYLE_USAGE ( .BOTH. , #520 ) ;
#6372 = EDGE_CURVE ( 'NONE', #3706, #8947, #1794, .T. ) ;
#6373 = ORIENTED_EDGE ( 'NONE', *, *, #1065, .F. ) ;
#6374 = CARTESIAN_POINT ( 'NONE',  ( 3.426491571325181340, 1.987932976489903636, -0.2209981660730357955 ) ) ;
#6375 = ORIENTED_EDGE ( 'NONE', *, *, #9707, .T. ) ;
#6376 = EDGE_CURVE ( 'NONE', #6614, #11155, #2786, .T. ) ;
#6377 = DIRECTION ( 'NONE',  ( -0.000000000000000000, -0.000000000000000000, -1.000000000000000000 ) ) ;
#6378 = EDGE_LOOP ( 'NONE', ( #3883, #11772 ) ) ;
#6379 = CARTESIAN_POINT ( 'NONE',  ( 0.7982897726210904654, -0.4436723967305212235, -0.3090191557806227785 ) ) ;
#6380 = CARTESIAN_POINT ( 'NONE',  ( 2.650000000000001688, 0.000000000000000000, 0.000000000000000000 ) ) ;
#6381 = CARTESIAN_POINT ( 'NONE',  ( -0.3724999999999999423, 0.000000000000000000, -0.4124999999999999778 ) ) ;
#6382 = CIRCLE ( 'NONE', #10531, 1.500000000000000222 ) ;
#6383 = DIRECTION ( 'NONE',  ( 0.000000000000000000, 0.7071067811865490160, 0.7071067811865459074 ) ) ;
#6384 = ORIENTED_EDGE ( 'NONE', *, *, #14019, .F. ) ;
#6385 = ORIENTED_EDGE ( 'NONE', *, *, #14185, .F. ) ;
#6386 = EDGE_LOOP ( 'NONE', ( #13070, #9194, #8642, #12618 ) ) ;
#6387 = EDGE_CURVE ( 'NONE', #7567, #14655, #4264, .T. ) ;
#6388 = EDGE_CURVE ( 'NONE', #1017, #10474, #4139, .T. ) ;
#6389 = CARTESIAN_POINT ( 'NONE',  ( 8.670688874134334867, 0.8757383175063406799, -0.2544954840226750781 ) ) ;
#6390 = ORIENTED_EDGE ( 'NONE', *, *, #4955, .F. ) ;
#6391 = PLANE ( 'NONE',  #13113 ) ;
#6392 = CARTESIAN_POINT ( 'NONE',  ( 2.124999999999999556, 1.575000000000000178, -2.360000000000016751 ) ) ;
#6393 = AXIS2_PLACEMENT_3D ( 'NONE', #9621, #4959, #323 ) ;
#6394 = DIRECTION ( 'NONE',  ( 0.000000000000000000, 1.000000000000000000, 0.000000000000000000 ) ) ;
#6395 = CARTESIAN_POINT ( 'NONE',  ( 3.923955648118384598, 1.840411246837426962, 0.7499999999999997780 ) ) ;
#6396 = PLANE ( 'NONE',  #10538 ) ;
#6397 = AXIS2_PLACEMENT_3D ( 'NONE', #10979, #4950, #5167 ) ;
#6398 = ORIENTED_EDGE ( 'NONE', *, *, #14156, .F. ) ;
#6399 = ORIENTED_EDGE ( 'NONE', *, *, #9452, .F. ) ;
#6400 = ORIENTED_EDGE ( 'NONE', *, *, #6008, .T. ) ;
#6401 = LINE ( 'NONE', #5246, #636 ) ;
#6402 = EDGE_CURVE ( 'NONE', #2606, #3991, #5204, .T. ) ;
#6403 = CARTESIAN_POINT ( 'NONE',  ( -0.2249147617188423653, 0.7512260236060024354, -0.3723417112827359654 ) ) ;
#6404 = CARTESIAN_POINT ( 'NONE',  ( 4.374208753957563367, 0.9996035968963620233, -0.03268784858779524849 ) ) ;
#6405 = ITEM_DEFINED_TRANSFORMATION ( 'NONE', 'NONE', #4749,  #8424 ) ;
#6406 = CARTESIAN_POINT ( 'NONE',  ( 0.3724999999999997757, -0.6290000000000003366, -0.3725000000000000533 ) ) ;
#6407 = ORIENTED_EDGE ( 'NONE', *, *, #1982, .F. ) ;
#6408 = DIRECTION ( 'NONE',  ( 0.000000000000000000, 0.000000000000000000, 1.000000000000000000 ) ) ;
#6409 = LINE ( 'NONE', #13273, #14632 ) ;
#6410 = CARTESIAN_POINT ( 'NONE',  ( 0.8999999999999998002, 0.000000000000000000, -0.2749999999999998557 ) ) ;
#6411 = CARTESIAN_POINT ( 'NONE',  ( 4.344846310392954436, 3.567999999999999616, 1.491010071662831393 ) ) ;
#6412 = CARTESIAN_POINT ( 'NONE',  ( 0.9254934464156098217, -0.4652881421103379767, -0.4458518134710270919 ) ) ;
#6413 = CARTESIAN_POINT ( 'NONE',  ( 4.497905261668263321, 1.733752379391429566, 0.4204404687884559788 ) ) ;
#6414 = EDGE_CURVE ( 'NONE', #114, #14916, #14496, .T. ) ;
#6416 = VERTEX_POINT ( 'NONE', #1742 ) ;
#6415 = DIRECTION ( 'NONE',  ( 0.000000000000000000, 0.000000000000000000, 1.000000000000000000 ) ) ;
#6417 = CIRCLE ( 'NONE', #10817, 1.500000000000000222 ) ;
#6418 = EDGE_CURVE ( 'NONE', #11005, #12302, #6432, .T. ) ;
#6419 = ORIENTED_EDGE ( 'NONE', *, *, #14722, .T. ) ;
#6420 = EDGE_CURVE ( 'NONE', #5828, #5637, #12554, .T. ) ;
#6421 = CARTESIAN_POINT ( 'NONE',  ( -0.2845281682845372528, 1.599152118624411756, -0.2690882622986915385 ) ) ;
#6423 = EDGE_LOOP ( 'NONE', ( #4526, #11807, #3427, #2355 ) ) ;
#6422 = FACE_OUTER_BOUND ( 'NONE', #5727, .T. ) ;
#6424 = ORIENTED_EDGE ( 'NONE', *, *, #4873, .T. ) ;
#6425 = CARTESIAN_POINT ( 'NONE',  ( 0.6653056208004448635, 0.01642763638135510268, 0.4725671546919802957 ) ) ;
#6426 =( NAMED_UNIT ( * ) SI_UNIT ( $, .STERADIAN. ) SOLID_ANGLE_UNIT ( ) );
#6427 = LINE ( 'NONE', #577, #1800 ) ;
#6428 = ORIENTED_EDGE ( 'NONE', *, *, #3071, .T. ) ;
#6429 = DIRECTION ( 'NONE',  ( -1.000000000000000000, 0.000000000000000000, -0.000000000000000000 ) ) ;
#6430 = LINE ( 'NONE', #6657, #13627 ) ;
#6431 = EDGE_CURVE ( 'NONE', #6255, #6090, #7914, .T. ) ;
#6432 = LINE ( 'NONE', #7903, #7441 ) ;
#6433 = CARTESIAN_POINT ( 'NONE',  ( 0.6732025385091793268, -0.04517367991929972099, 0.4888865340280583727 ) ) ;
#6434 = CARTESIAN_POINT ( 'NONE',  ( 0.9705801008103163152, -0.4829849771478168519, -0.3489154846764306872 ) ) ;
#6435 = ORIENTED_EDGE ( 'NONE', *, *, #1083, .F. ) ;
#6436 = CARTESIAN_POINT ( 'NONE',  ( 2.807059454666800402, 0.6196377705552925663, 0.4603522675894519689 ) ) ;
#6437 = AXIS2_PLACEMENT_3D ( 'NONE', #4240, #3008, #4961 ) ;
#6438 = DIRECTION ( 'NONE',  ( 0.000000000000000000, 0.000000000000000000, 1.000000000000000000 ) ) ;
#6439 = EDGE_CURVE ( 'NONE', #14916, #114, #5969, .T. ) ;
#6440 = ORIENTED_EDGE ( 'NONE', *, *, #11951, .F. ) ;
#6441 = LINE ( 'NONE', #10041, #8924 ) ;
#6442 = CARTESIAN_POINT ( 'NONE',  ( 3.874999999999999556, 3.567999999999999616, -1.320000000000000062 ) ) ;
#6443 = VERTEX_POINT ( 'NONE', #5098 ) ;
#6444 = CARTESIAN_POINT ( 'NONE',  ( 2.774999999999999911, 0.9800000000000039790, 3.360000000000000320 ) ) ;
#6445 = ORIENTED_EDGE ( 'NONE', *, *, #519, .F. ) ;
#6446 = SURFACE_SIDE_STYLE ('',( #13693 ) ) ;
#6447 = CONICAL_SURFACE ( 'NONE', #8173, 2.960629921259841257, 0.7853981633974552734 ) ;
#6448 = CARTESIAN_POINT ( 'NONE',  ( 0.6179999999999965521, -1.679378605318047946, -1.304378605318053053 ) ) ;
#6449 = ADVANCED_FACE ( 'NONE', ( #14410 ), #9643, .F. ) ;
#6450 = CIRCLE ( 'NONE', #8417, 0.7500000000000001110 ) ;
#6451 = CARTESIAN_POINT ( 'NONE',  ( 0.8337711728933204780, -0.4835921594977613536, -0.3396201722514596288 ) ) ;
#6452 = EDGE_CURVE ( 'NONE', #4181, #4765, #11086, .T. ) ;
#6453 = DIRECTION ( 'NONE',  ( 0.000000000000000000, 0.000000000000000000, -1.000000000000000000 ) ) ;
#6454 =( NAMED_UNIT ( * ) PLANE_ANGLE_UNIT ( ) SI_UNIT ( $, .RADIAN. ) );
#6455 = VECTOR ( 'NONE', #9869, 39.37007874015748143 ) ;
#6456 = CYLINDRICAL_SURFACE ( 'NONE', #3755, 0.7849999999999969225 ) ;
#6457 = ORIENTED_EDGE ( 'NONE', *, *, #9342, .T. ) ;
#6458 = ORIENTED_EDGE ( 'NONE', *, *, #896, .T. ) ;
#6459 = VERTEX_POINT ( 'NONE', #12696 ) ;
#6460 = CIRCLE ( 'NONE', #9146, 0.07500000000000002498 ) ;
#6461 = DIRECTION ( 'NONE',  ( 0.000000000000000000, 0.000000000000000000, -1.000000000000000000 ) ) ;
#6462 = ORIENTED_EDGE ( 'NONE', *, *, #1918, .T. ) ;
#6463 = CARTESIAN_POINT ( 'NONE',  ( 0.6412116890856961460, -0.6589999999999996971, 8.478919399169820819E-17 ) ) ;
#6464 = CARTESIAN_POINT ( 'NONE',  ( 2.599160627732593376, 0.7974701832127791823, 0.4632886916986920789 ) ) ;
#6465 = DIRECTION ( 'NONE',  ( 0.000000000000000000, 1.000000000000000000, -1.423315761404775650E-14 ) ) ;
#6466 = AXIS2_PLACEMENT_3D ( 'NONE', #11275, #10135, #14645 ) ;
#6467 = CARTESIAN_POINT ( 'NONE',  ( 4.439088310279003302, 1.783130252920299696, 0.4984960193556706720 ) ) ;
#6468 = EDGE_CURVE ( 'NONE', #8487, #3272, #3033, .T. ) ;
#6469 = EDGE_CURVE ( 'NONE', #5312, #7123, #3219, .T. ) ;
#6470 = ORIENTED_EDGE ( 'NONE', *, *, #4086, .F. ) ;
#6471 = EDGE_LOOP ( 'NONE', ( #13179, #9468, #3005, #4300, #5954, #5639, #1988, #11130 ) ) ;
#6472 = ORIENTED_EDGE ( 'NONE', *, *, #236, .T. ) ;
#6473 = AXIS2_PLACEMENT_3D ( 'NONE', #9843, #8563, #8697 ) ;
#6474 = VERTEX_POINT ( 'NONE', #10189 ) ;
#6475 = DIRECTION ( 'NONE',  ( 0.000000000000000000, 0.000000000000000000, -1.000000000000000000 ) ) ;
#6476 = CONICAL_SURFACE ( 'NONE', #2805, 0.4070000000000022489, 0.7853981633974547183 ) ;
#6477 = AXIS2_PLACEMENT_3D ( 'NONE', #1070, #10423, #4235 ) ;
#6478 = CARTESIAN_POINT ( 'NONE',  ( 4.344846310392954436, 2.750000000000000000, 1.491010071662831171 ) ) ;
#6479 = CARTESIAN_POINT ( 'NONE',  ( 3.941521638426727758, 0.8684168616498817439, 0.4958385474027912632 ) ) ;
#6480 = DIRECTION ( 'NONE',  ( 1.000000000000000000, 0.000000000000000000, 0.000000000000000000 ) ) ;
#6481 = ORIENTED_EDGE ( 'NONE', *, *, #6468, .T. ) ;
#6482 = CARTESIAN_POINT ( 'NONE',  ( 2.124999999999999556, 2.359999999999999876, -1.575000000000016831 ) ) ;
#6483 = DIRECTION ( 'NONE',  ( 0.03489949670249522379, -0.9993908270190959842, 0.000000000000000000 ) ) ;
#6484 = DIRECTION ( 'NONE',  ( 0.000000000000000000, 0.000000000000000000, 1.000000000000000000 ) ) ;
#6485 = EDGE_CURVE ( 'NONE', #12151, #7622, #13606, .T. ) ;
#6486 = CIRCLE ( 'NONE', #6744, 0.4349999999999999423 ) ;
#6487 = EDGE_CURVE ( 'NONE', #4855, #3137, #13684, .T. ) ;
#6488 = CARTESIAN_POINT ( 'NONE',  ( 8.849999999999999645, 0.9399413264884247665, 6.829619984160658046E-17 ) ) ;
#6489 = AXIS2_PLACEMENT_3D ( 'NONE', #5276, #1740, #10101 ) ;
#6490 = AXIS2_PLACEMENT_3D ( 'NONE', #9719, #4982, #9578 ) ;
#6491 = CARTESIAN_POINT ( 'NONE',  ( 0.9618623841134203989, -0.4823031615770373981, -0.4179641926583888001 ) ) ;
#6492 = CARTESIAN_POINT ( 'NONE',  ( 4.593106923254413942, 1.719712382094653824, 0.3671620375188934804 ) ) ;
#6494 = ORIENTED_EDGE ( 'NONE', *, *, #9889, .T. ) ;
#6493 = DIRECTION ( 'NONE',  ( 0.000000000000000000, 0.000000000000000000, 1.000000000000000000 ) ) ;
#6495 = ORIENTED_EDGE ( 'NONE', *, *, #10574, .F. ) ;
#6497 = ORIENTED_EDGE ( 'NONE', *, *, #11689, .F. ) ;
#6496 = CARTESIAN_POINT ( 'NONE',  ( 0.3724999999999999423, -0.6590000000000000302, 0.4124999999999999223 ) ) ;
#6498 = ORIENTED_EDGE ( 'NONE', *, *, #14133, .F. ) ;
#6499 = CARTESIAN_POINT ( 'NONE',  ( 0.8999999999999999112, -0.6429999999999999050, -0.3750000000000000555 ) ) ;
#6500 = AXIS2_PLACEMENT_3D ( 'NONE', #14368, #652, #14595 ) ;
#6501 = FACE_OUTER_BOUND ( 'NONE', #10469, .T. ) ;
#6502 = ORIENTED_EDGE ( 'NONE', *, *, #1157, .F. ) ;
#6503 = FACE_OUTER_BOUND ( 'NONE', #3409, .T. ) ;
#6504 = DIRECTION ( 'NONE',  ( 0.000000000000000000, 0.000000000000000000, 1.000000000000000000 ) ) ;
#6505 = AXIS2_PLACEMENT_3D ( 'NONE', #14503, #15027, #13579 ) ;
#6506 = VECTOR ( 'NONE', #12653, 39.37007874015748143 ) ;
#6507 = DIRECTION ( 'NONE',  ( 0.000000000000000000, 0.000000000000000000, -1.000000000000000000 ) ) ;
#6508 = EDGE_CURVE ( 'NONE', #6847, #4204, #14551, .T. ) ;
#6509 = CARTESIAN_POINT ( 'NONE',  ( 2.187631780374527324, 0.4716415227047954795, -0.4691012460399074380 ) ) ;
#6510 = CARTESIAN_POINT ( 'NONE',  ( 1.003096136995459631, -0.4429976034824906761, -0.4258273028168332863 ) ) ;
#6511 = ORIENTED_EDGE ( 'NONE', *, *, #11090, .T. ) ;
#6512 = AXIS2_PLACEMENT_3D ( 'NONE', #9790, #7635, #2899 ) ;
#6513 = CARTESIAN_POINT ( 'NONE',  ( 0.000000000000000000, 0.000000000000000000, 0.000000000000000000 ) ) ;
#6514 = CARTESIAN_POINT ( 'NONE',  ( 2.980731298636167370, 3.567999999999999616, 0.3249191361593796734 ) ) ;
#6515 = ORIENTED_EDGE ( 'NONE', *, *, #7688, .T. ) ;
#6516 = CARTESIAN_POINT ( 'NONE',  ( 0.7176122613104018999, -0.4347745074854311165, 0.4611624156322181034 ) ) ;
#6517 = DIRECTION ( 'NONE',  ( 0.000000000000000000, 0.000000000000000000, 1.000000000000000000 ) ) ;
#6518 = EDGE_LOOP ( 'NONE', ( #5807, #8928, #599, #6580, #7505, #10733 ) ) ;
#6519 = CARTESIAN_POINT ( 'NONE',  ( 6.826491571325181695, 1.679378605318059492, 2.086378605318041757 ) ) ;
#6520 = ORIENTED_EDGE ( 'NONE', *, *, #8940, .F. ) ;
#6521 =( LENGTH_UNIT ( ) NAMED_UNIT ( * ) SI_UNIT ( $, .METRE. ) );
#6522 = CONICAL_SURFACE ( 'NONE', #10432, 0.6412116890856960350, 1.326062729686469988 ) ;
#6523 = DIRECTION ( 'NONE',  ( -0.000000000000000000, 1.000000000000000000, -0.000000000000000000 ) ) ;
#6524 = EDGE_CURVE ( 'NONE', #3025, #3922, #6955, .T. ) ;
#6525 = EDGE_CURVE ( 'NONE', #10348, #14590, #13753, .T. ) ;
#6526 = FACE_OUTER_BOUND ( 'NONE', #11284, .T. ) ;
#6527 = CARTESIAN_POINT ( 'NONE',  ( 0.7859940414473148840, -0.4452037809602719665, -0.3216753057612609656 ) ) ;
#6528 = EDGE_CURVE ( 'NONE', #5693, #8959, #3294, .T. ) ;
#6529 = CARTESIAN_POINT ( 'NONE',  ( 0.9666439951188899871, -0.4829990579840729437, -0.4094329656214278912 ) ) ;
#6530 = VERTEX_POINT ( 'NONE', #7962 ) ;
#6531 = CARTESIAN_POINT ( 'NONE',  ( 3.061616997868382402E-17, 0.04580000000000046534, 0.2499999999999999167 ) ) ;
#6532 = CARTESIAN_POINT ( 'NONE',  ( 3.504516174824143793, 1.917097053177361010, 0.7259348004102793572 ) ) ;
#6533 = ADVANCED_FACE ( 'NONE', ( #14842 ), #4375, .T. ) ;
#6534 = CIRCLE ( 'NONE', #11348, 0.2945000000000009277 ) ;
#6535 = CARTESIAN_POINT ( 'NONE',  ( 0.1007315414569005807, 0.1749999999999999889, -0.7936328852534507705 ) ) ;
#6536 = ORIENTED_EDGE ( 'NONE', *, *, #6754, .T. ) ;
#6537 = ORIENTED_EDGE ( 'NONE', *, *, #8940, .T. ) ;
#6538 = EDGE_CURVE ( 'NONE', #4204, #1773, #7614, .T. ) ;
#6539 = DIRECTION ( 'NONE',  ( 0.000000000000000000, 0.000000000000000000, -1.000000000000000000 ) ) ;
#6540 = ORIENTED_EDGE ( 'NONE', *, *, #9380, .F. ) ;
#6541 = FACE_OUTER_BOUND ( 'NONE', #6599, .T. ) ;
#6542 = CONICAL_SURFACE ( 'NONE', #2863, 0.2224999999999996148, 0.7853981633974446153 ) ;
#6543 = CARTESIAN_POINT ( 'NONE',  ( 0.7009834207394823880, -0.3992359203334029383, -0.4880078140243664930 ) ) ;
#6544 = PRODUCT ( 'Thermostate Flange', 'Thermostate Flange', '', ( #2666 ) ) ;
#6545 = CARTESIAN_POINT ( 'NONE',  ( 3.426491571325181340, 2.062169880637645836, -0.5999481385559802815 ) ) ;
#6546 = CARTESIAN_POINT ( 'NONE',  ( 4.100009802906539491, 1.799994069799653484, 0.7160437602263716173 ) ) ;
#6547 = VECTOR ( 'NONE', #14405, 39.37007874015748854 ) ;
#6548 = VERTEX_POINT ( 'NONE', #57 ) ;
#6549 = AXIS2_PLACEMENT_3D ( 'NONE', #4683, #10794, #3836 ) ;
#6550 = ADVANCED_FACE ( 'NONE', ( #15149 ), #4599, .F. ) ;
#6551 = ORIENTED_EDGE ( 'NONE', *, *, #11180, .F. ) ;
#6552 = ORIENTED_EDGE ( 'NONE', *, *, #6862, .F. ) ;
#6553 = EDGE_CURVE ( 'NONE', #3706, #5573, #13911, .T. ) ;
#6554 = VERTEX_POINT ( 'NONE', #11633 ) ;
#6555 = CIRCLE ( 'NONE', #4362, 0.7500000000000001110 ) ;
#6556 = DIRECTION ( 'NONE',  ( -0.000000000000000000, 4.591341165821852610E-16, -1.000000000000000000 ) ) ;
#6557 = LINE ( 'NONE', #11217, #11530 ) ;
#6559 = CIRCLE ( 'NONE', #10226, 0.03999999999999998695 ) ;
#6558 = CARTESIAN_POINT ( 'NONE',  ( 2.774999999999999911, -2.360000000000000320, 1.575000000000016387 ) ) ;
#6560 = EDGE_CURVE ( 'NONE', #10623, #7355, #13763, .T. ) ;
#6561 = CARTESIAN_POINT ( 'NONE',  ( 0.2099999999999999922, 1.559103846021543172, -0.3809527529760087239 ) ) ;
#6562 = ORIENTED_EDGE ( 'NONE', *, *, #9096, .F. ) ;
#6563 = CARTESIAN_POINT ( 'NONE',  ( 0.7067472695984847730, -0.05999999999999996309, 0.5500236785040135690 ) ) ;
#6564 = CARTESIAN_POINT ( 'NONE',  ( 8.849152626892301754, -0.3829999999999988414, 0.3150059839749300705 ) ) ;
#6565 = CARTESIAN_POINT ( 'NONE',  ( 2.743000000000000771, 1.679378605318059048, 1.941878605318041240 ) ) ;
#6566 = DIRECTION ( 'NONE',  ( 1.000000000000000000, 0.000000000000000000, 0.000000000000000000 ) ) ;
#6567 = VECTOR ( 'NONE', #13766, 39.37007874015748143 ) ;
#6568 = AXIS2_PLACEMENT_3D ( 'NONE', #4371, #7733, #12387 ) ;
#6569 = MECHANICAL_DESIGN_GEOMETRIC_PRESENTATION_REPRESENTATION (  '', ( #10969 ), #12668 ) ;
#6570 = DIRECTION ( 'NONE',  ( -0.9999002670844989726, -0.000000000000000000, -0.01412288512831212997 ) ) ;
#6571 = AXIS2_PLACEMENT_3D ( 'NONE', #14138, #7125, #2518 ) ;
#6572 = CARTESIAN_POINT ( 'NONE',  ( 0.8920597045391224222, -0.4611706669540619474, -0.4498866585187662470 ) ) ;
#6573 = CARTESIAN_POINT ( 'NONE',  ( 3.858712094495529321, 1.861610320989349754, 0.7499885605692133694 ) ) ;
#6575 = VERTEX_POINT ( 'NONE', #10710 ) ;
#6574 = CARTESIAN_POINT ( 'NONE',  ( 3.875000000000000000, 1.885381157978844868, -0.5000000000000002220 ) ) ;
#6576 = ORIENTED_EDGE ( 'NONE', *, *, #12725, .F. ) ;
#6578 = ORIENTED_EDGE ( 'NONE', *, *, #12613, .F. ) ;
#6577 = DIRECTION ( 'NONE',  ( -1.000000000000000000, 0.000000000000000000, 0.000000000000000000 ) ) ;
#6579 = AXIS2_PLACEMENT_3D ( 'NONE', #1900, #586, #816 ) ;
#6580 = ORIENTED_EDGE ( 'NONE', *, *, #6388, .T. ) ;
#6581 = DIRECTION ( 'NONE',  ( 0.000000000000000000, 0.000000000000000000, -1.000000000000000000 ) ) ;
#6582 = ADVANCED_FACE ( 'NONE', ( #4829 ), #14063, .F. ) ;
#6583 = FACE_OUTER_BOUND ( 'NONE', #13043, .T. ) ;
#6584 = EDGE_LOOP ( 'NONE', ( #379, #3485, #578, #9295 ) ) ;
#6585 = VECTOR ( 'NONE', #9047, 39.37007874015748143 ) ;
#6586 = LINE ( 'NONE', #234, #14535 ) ;
#6587 = DIRECTION ( 'NONE',  ( -0.000000000000000000, -0.000000000000000000, -1.000000000000000000 ) ) ;
#6588 = VECTOR ( 'NONE', #7252, 39.37007874015748143 ) ;
#6589 = DIRECTION ( 'NONE',  ( 0.000000000000000000, 0.000000000000000000, -1.000000000000000000 ) ) ;
#6590 = ORIENTED_EDGE ( 'NONE', *, *, #8313, .T. ) ;
#6591 = CIRCLE ( 'NONE', #13171, 0.4070000000000055240 ) ;
#6592 = CARTESIAN_POINT ( 'NONE',  ( 3.388933043275772494, 0.7513023213622327390, 0.4521337140780258279 ) ) ;
#6593 = CARTESIAN_POINT ( 'NONE',  ( 3.388178971404831596, 0.9934719948626907771, 0.1152309124458658768 ) ) ;
#6594 = CARTESIAN_POINT ( 'NONE',  ( 4.430922016235464334, 1.707647511453724842, -0.5743937140048646084 ) ) ;
#6595 = ORIENTED_EDGE ( 'NONE', *, *, #308, .F. ) ;
#6596 = CIRCLE ( 'NONE', #12697, 0.1050000000000001071 ) ;
#6597 = CARTESIAN_POINT ( 'NONE',  ( 4.180700663235655590, 0.9180451591693143953, -0.3969666424556979045 ) ) ;
#6598 = DIRECTION ( 'NONE',  ( 0.000000000000000000, -1.000000000000000000, 0.000000000000000000 ) ) ;
#6599 = EDGE_LOOP ( 'NONE', ( #8030, #4818, #8796, #7834 ) ) ;
#6600 = DIRECTION ( 'NONE',  ( 0.000000000000000000, 0.000000000000000000, -1.000000000000000000 ) ) ;
#6601 = VERTEX_POINT ( 'NONE', #3604 ) ;
#6602 = ADVANCED_FACE ( 'NONE', ( #2454, #7134, #13064, #5971, #14148, #11003 ), #8636, .F. ) ;
#6603 = CARTESIAN_POINT ( 'NONE',  ( 4.769268701363833074, 3.567999999999999616, -0.3249191361593797289 ) ) ;
#6604 = CARTESIAN_POINT ( 'NONE',  ( 3.458450979136563852, 2.043671318866147946, -0.6239234495429138994 ) ) ;
#6605 = AXIS2_PLACEMENT_3D ( 'NONE', #4973, #8490, #8567 ) ;
#6606 = CARTESIAN_POINT ( 'NONE',  ( 2.219979583768778131, -0.03321525116820610996, 0.4091553120912245212 ) ) ;
#6607 = DIRECTION ( 'NONE',  ( 0.000000000000000000, 1.000000000000000000, -0.000000000000000000 ) ) ;
#6608 = DIRECTION ( 'NONE',  ( -1.000000000000000000, -0.000000000000000000, -0.000000000000000000 ) ) ;
#6609 = CARTESIAN_POINT ( 'NONE',  ( 2.742999999999998995, -1.679378605318059048, -1.941878605318027251 ) ) ;
#6610 = EDGE_LOOP ( 'NONE', ( #12997, #2464, #8904, #6921 ) ) ;
#6611 = DIRECTION ( 'NONE',  ( 0.000000000000000000, 0.000000000000000000, -1.000000000000000000 ) ) ;
#6612 = DIRECTION ( 'NONE',  ( 0.000000000000000000, 0.000000000000000000, 1.000000000000000000 ) ) ;
#6613 = CARTESIAN_POINT ( 'NONE',  ( 0.7020310496751531737, -0.4139656494879343507, -0.4816878228448813193 ) ) ;
#6614 = VERTEX_POINT ( 'NONE', #5053 ) ;
#6615 = VERTEX_POINT ( 'NONE', #13139 ) ;
#6616 = EDGE_CURVE ( 'NONE', #2859, #3525, #7202, .T. ) ;
#6617 = EDGE_CURVE ( 'NONE', #7135, #6235, #3274, .T. ) ;
#6618 = LINE ( 'NONE', #7904, #6269 ) ;
#6619 = ORIENTED_EDGE ( 'NONE', *, *, #11706, .F. ) ;
#6620 = EDGE_CURVE ( 'NONE', #327, #2972, #7562, .T. ) ;
#6621 = CARTESIAN_POINT ( 'NONE',  ( 0.09500000000000431710, -1.679378605318047946, -1.304378605318053053 ) ) ;
#6622 = CARTESIAN_POINT ( 'NONE',  ( 0.7022453151856608011, -0.4144781913240899729, -0.4813241942165185638 ) ) ;
#6623 = DIRECTION ( 'NONE',  ( -1.000000000000000000, -0.000000000000000000, -0.000000000000000000 ) ) ;
#6624 = EDGE_CURVE ( 'NONE', #7356, #8150, #12071, .T. ) ;
#6625 = DIRECTION ( 'NONE',  ( 1.000000000000000000, 0.000000000000000000, 0.000000000000000000 ) ) ;
#6626 = CIRCLE ( 'NONE', #14190, 0.4349999999999999423 ) ;
#6627 = ORIENTED_EDGE ( 'NONE', *, *, #7011, .T. ) ;
#6628 = B_SPLINE_CURVE_WITH_KNOTS ( 'NONE', 3,
 ( #11676, #13030, #1101, #1252, #5938, #8092, #1179, #175, #7021, #12733, #2258, #3722, #25, #3488, #14187, #8167, #11595, #2340, #2494, #10601 ),
 .UNSPECIFIED., .F., .F.,
 ( 4, 2, 2, 2, 2, 2, 2, 2, 2, 4 ),
 ( 0.000000000000000000, 0.0005275929577467031390, 0.001055185915493406278, 0.001582778873240109525, 0.002110371830986812556, 0.002374168309860159084, 0.002637964788733505178, 0.003165557746480196499, 0.003693150704226888254, 0.004220743661973579142 ),
 .UNSPECIFIED. ) ;
#6629 = VERTEX_POINT ( 'NONE', #14440 ) ;
#6630 = ORIENTED_EDGE ( 'NONE', *, *, #11883, .T. ) ;
#6631 = ORIENTED_EDGE ( 'NONE', *, *, #6804, .T. ) ;
#6632 = AXIS2_PLACEMENT_3D ( 'NONE', #2318, #7000, #5854 ) ;
#6633 = CARTESIAN_POINT ( 'NONE',  ( 0.000000000000000000, 1.000000000000000000, 0.000000000000000000 ) ) ;
#6634 = DIRECTION ( 'NONE',  ( 0.000000000000000000, 0.000000000000000000, -1.000000000000000000 ) ) ;
#6635 = LINE ( 'NONE', #13570, #3408 ) ;
#6636 = CARTESIAN_POINT ( 'NONE',  ( 3.874999999999999556, 2.782000000000002693, 1.130000000000000560 ) ) ;
#6637 = EDGE_LOOP ( 'NONE', ( #10117, #1755, #5164, #6631 ) ) ;
#6638 = CARTESIAN_POINT ( 'NONE',  ( 3.102108017520303740, 0.6812791890164018316, 0.3964255093850733713 ) ) ;
#6639 = DIRECTION ( 'NONE',  ( 0.000000000000000000, 0.000000000000000000, -1.000000000000000000 ) ) ;
#6640 = CARTESIAN_POINT ( 'NONE',  ( 0.000000000000000000, 1.559103846021539619, 0.000000000000000000 ) ) ;
#6641 = EDGE_CURVE ( 'NONE', #12484, #8434, #13353, .T. ) ;
#6642 = AXIS2_PLACEMENT_3D ( 'NONE', #395, #5237, #4013 ) ;
#6643 = CARTESIAN_POINT ( 'NONE',  ( 0.9056315879401858338, -0.4606766705580153110, -0.4500955733274891180 ) ) ;
#6644 = ADVANCED_FACE ( 'NONE', ( #10857 ), #10933, .F. ) ;
#6645 = CARTESIAN_POINT ( 'NONE',  ( 4.525494676330790611, 1.792733192933819053, 0.3777435136916634795 ) ) ;
#6647 = ORIENTED_EDGE ( 'NONE', *, *, #4667, .T. ) ;
#6646 = CARTESIAN_POINT ( 'NONE',  ( 3.693802410306114226, 1.943924811042458733, -0.4665840092633480318 ) ) ;
#6648 = EDGE_LOOP ( 'NONE', ( #12960, #614, #5197, #10864 ) ) ;
#6650 = ORIENTED_EDGE ( 'NONE', *, *, #10501, .T. ) ;
#6649 = DIRECTION ( 'NONE',  ( 0.000000000000000000, 0.000000000000000000, -1.000000000000000000 ) ) ;
#6651 = EDGE_LOOP ( 'NONE', ( #14747, #11543, #9126, #732 ) ) ;
#6652 = DIRECTION ( 'NONE',  ( -0.7071067811865421326, 8.659560562354996953E-17, -0.7071067811865527908 ) ) ;
#6653 = LENGTH_MEASURE_WITH_UNIT ( LENGTH_MEASURE( 0.02539999999999999897 ), #7572 );
#6654 = DIRECTION ( 'NONE',  ( -1.000000000000000000, -0.000000000000000000, -0.000000000000000000 ) ) ;
#6655 = ORIENTED_EDGE ( 'NONE', *, *, #1283, .F. ) ;
#6656 = CARTESIAN_POINT ( 'NONE',  ( 0.2249147617188371751, 0.7512260236060024354, -0.3723417112827391295 ) ) ;
#6657 = CARTESIAN_POINT ( 'NONE',  ( 2.088340948482054316, 0.2866505039622389006, 0.4705036589197449937 ) ) ;
#6658 = LINE ( 'NONE', #13519, #1089 ) ;
#6659 = CARTESIAN_POINT ( 'NONE',  ( 0.9719779994246295907, -0.4829746353139036663, -0.3969404040289119528 ) ) ;
#6660 = CIRCLE ( 'NONE', #4228, 0.7500000000000001110 ) ;
#6661 = EDGE_CURVE ( 'NONE', #8969, #4411, #2302, .T. ) ;
#6662 = ORIENTED_EDGE ( 'NONE', *, *, #260, .T. ) ;
#6663 = ADVANCED_FACE ( 'NONE', ( #6352 ), #5128, .F. ) ;
#6664 = DIRECTION ( 'NONE',  ( -0.2588190451024959260, 0.000000000000000000, 0.9659258262890748625 ) ) ;
#6665 = CARTESIAN_POINT ( 'NONE',  ( 3.441951518218600015, 0.9681238899719051272, -0.2520395006946318239 ) ) ;
#6666 = DIRECTION ( 'NONE',  ( -0.000000000000000000, 1.000000000000000000, -0.000000000000000000 ) ) ;
#6667 = CARTESIAN_POINT ( 'NONE',  ( 0.7096982392392976458, -0.4275148688008855724, 0.4703908291968755262 ) ) ;
#6668 = CARTESIAN_POINT ( 'NONE',  ( 0.2849999999999999756, 4.529999999999999361, 0.4108223460329293864 ) ) ;
#6669 = ORIENTED_EDGE ( 'NONE', *, *, #916, .F. ) ;
#6670 = CONICAL_SURFACE ( 'NONE', #51, 0.2224999999999996148, 0.7853981633974446153 ) ;
#6671 = CARTESIAN_POINT ( 'NONE',  ( 0.9708583742000757022, -0.4829832308505582206, -0.3495890805477908647 ) ) ;
#6672 = EDGE_LOOP ( 'NONE', ( #11207, #2640, #7941, #9193 ) ) ;
#6673 = CARTESIAN_POINT ( 'NONE',  ( 3.875000000000000000, 3.535499999999999865, 0.000000000000000000 ) ) ;
#6674 = CONICAL_SURFACE ( 'NONE', #776, 0.2225000000000012523, 0.7853981633974446153 ) ;
#6675 = CARTESIAN_POINT ( 'NONE',  ( 2.702105678820072132, 0.5048229836667897930, -0.4618346655533888123 ) ) ;
#6676 = CARTESIAN_POINT ( 'NONE',  ( 0.6922886459387327385, -0.4439147467600604857, -0.4416098182902895575 ) ) ;
#6677 = CARTESIAN_POINT ( 'NONE',  ( 2.124999999999999556, 0.000000000000000000, 0.000000000000000000 ) ) ;
#6678 = AXIS2_PLACEMENT_3D ( 'NONE', #12589, #4809, #12900 ) ;
#6679 = DIRECTION ( 'NONE',  ( -1.365923996832131609E-16, 1.000000000000000000, 0.000000000000000000 ) ) ;
#6680 = ORIENTED_EDGE ( 'NONE', *, *, #2418, .F. ) ;
#6681 = CARTESIAN_POINT ( 'NONE',  ( 3.426491571325181340, -0.9799999999999436939, 3.360000000000016751 ) ) ;
#6682 = CARTESIAN_POINT ( 'NONE',  ( 3.828636530710406216, 1.793264967391777542, 0.7984341528290008760 ) ) ;
#6683 = CARTESIAN_POINT ( 'NONE',  ( 0.7174986153957904067, -0.4347107752510870893, -0.4612806347796395978 ) ) ;
#6684 = ORIENTED_EDGE ( 'NONE', *, *, #4290, .F. ) ;
#6685 = ORIENTED_EDGE ( 'NONE', *, *, #2219, .T. ) ;
#6686 = DIRECTION ( 'NONE',  ( -1.000000000000000000, -0.000000000000000000, -0.000000000000000000 ) ) ;
#6687 = VERTEX_POINT ( 'NONE', #14508 ) ;
#6688 = VECTOR ( 'NONE', #6735, 39.37007874015748143 ) ;
#6689 = CARTESIAN_POINT ( 'NONE',  ( 3.405153689607044232, 3.567999999999999616, 1.491010071662831171 ) ) ;
#6690 = PLANE ( 'NONE',  #8115 ) ;
#6691 = DIRECTION ( 'NONE',  ( 1.000000000000000000, 0.000000000000000000, 0.000000000000000000 ) ) ;
#6692 = CARTESIAN_POINT ( 'NONE',  ( 3.537411752015444222, 2.007197475989087820, 0.3717360073472075199 ) ) ;
#6693 = EDGE_CURVE ( 'NONE', #14527, #8165, #4042, .T. ) ;
#6694 = VERTEX_POINT ( 'NONE', #9717 ) ;
#6695 = AXIS2_PLACEMENT_3D ( 'NONE', #2449, #10782, #12816 ) ;
#6696 = AXIS2_PLACEMENT_3D ( 'NONE', #13048, #2514, #3741 ) ;
#6697 = EDGE_LOOP ( 'NONE', ( #8499, #2624 ) ) ;
#6698 = ORIENTED_EDGE ( 'NONE', *, *, #6196, .T. ) ;
#6699 = EDGE_CURVE ( 'NONE', #1776, #5690, #11070, .T. ) ;
#6700 = DIRECTION ( 'NONE',  ( -1.000000000000000000, -0.000000000000000000, -0.000000000000000000 ) ) ;
#6701 = ORIENTED_EDGE ( 'NONE', *, *, #9911, .T. ) ;
#6702 = DIRECTION ( 'NONE',  ( 0.000000000000000000, -1.000000000000000000, 0.000000000000000000 ) ) ;
#6703 = DIRECTION ( 'NONE',  ( -0.000000000000000000, -1.000000000000000000, -0.000000000000000000 ) ) ;
#6704 = CARTESIAN_POINT ( 'NONE',  ( 0.7827579871403669287, -0.4452001257954049107, -0.3294746359414947312 ) ) ;
#6705 = CARTESIAN_POINT ( 'NONE',  ( 0.01818920831125209192, 1.603403463250998584, -0.3809527529760088904 ) ) ;
#6706 = EDGE_LOOP ( 'NONE', ( #11027, #10793, #11863, #6725, #10569 ) ) ;
#6707 = VECTOR ( 'NONE', #4348, 39.37007874015748143 ) ;
#6708 = CARTESIAN_POINT ( 'NONE',  ( 3.133380147778130453, 2.497928943106615396, 0.1166857200839504505 ) ) ;
#6709 = CARTESIAN_POINT ( 'NONE',  ( 0.6558215032554000068, -0.01848230360567671218, -0.5012403847680007019 ) ) ;
#6710 = CARTESIAN_POINT ( 'NONE',  ( 2.774999999999999911, -0.9799999999999989830, -2.359999999999999876 ) ) ;
#6711 = DIRECTION ( 'NONE',  ( 0.000000000000000000, 1.000000000000000000, 0.000000000000000000 ) ) ;
#6712 = EDGE_CURVE ( 'NONE', #2844, #10000, #14020, .T. ) ;
#6713 = EDGE_CURVE ( 'NONE', #3499, #14976, #9405, .T. ) ;
#6714 = CARTESIAN_POINT ( 'NONE',  ( 0.8874725658679039064, -0.4299024001883317569, -0.4648823484497104364 ) ) ;
#6715 = AXIS2_PLACEMENT_3D ( 'NONE', #2689, #12639, #8368 ) ;
#6716 = CARTESIAN_POINT ( 'NONE',  ( 4.391810419801174703, 1.780532734934683337, 0.5461860461645056120 ) ) ;
#6717 = CIRCLE ( 'NONE', #14523, 0.4070000000000025264 ) ;
#6719 = ORIENTED_EDGE ( 'NONE', *, *, #8746, .T. ) ;
#6718 = CARTESIAN_POINT ( 'NONE',  ( 3.426491571325181340, 1.954234464180151676, -0.6847610993685215863 ) ) ;
#6720 = AXIS2_PLACEMENT_3D ( 'NONE', #11496, #4532, #913 ) ;
#6721 = B_SPLINE_CURVE_WITH_KNOTS ( 'NONE', 3,
 ( #4342, #2345, #7026, #9014 ),
 .UNSPECIFIED., .F., .F.,
 ( 4, 4 ),
 ( 0.000000000000000000, 0.0001180456142323141122 ),
 .UNSPECIFIED. ) ;
#6722 = EDGE_CURVE ( 'NONE', #10316, #13316, #2047, .T. ) ;
#6723 = ORIENTED_EDGE ( 'NONE', *, *, #4311, .F. ) ;
#6725 = ORIENTED_EDGE ( 'NONE', *, *, #9608, .F. ) ;
#6724 = CARTESIAN_POINT ( 'NONE',  ( 0.6500000000000001332, 0.000000000000000000, 0.000000000000000000 ) ) ;
#6726 = VERTEX_POINT ( 'NONE', #11930 ) ;
#6727 = EDGE_CURVE ( 'NONE', #14371, #13066, #9935, .T. ) ;
#6728 = LINE ( 'NONE', #3356, #2885 ) ;
#6729 =( CONVERSION_BASED_UNIT ( 'INCH', #658 ) LENGTH_UNIT ( ) NAMED_UNIT ( #7450 ) );
#6730 = CARTESIAN_POINT ( 'NONE',  ( 2.774999999999999911, 1.679378605318042395, -1.679378605318058604 ) ) ;
#6731 = ORIENTED_EDGE ( 'NONE', *, *, #12482, .T. ) ;
#6732 = DIRECTION ( 'NONE',  ( 0.7071067811865421326, 8.659560562354996953E-17, 0.7071067811865527908 ) ) ;
#6733 = CARTESIAN_POINT ( 'NONE',  ( 3.875000000000000000, 3.137999999999999901, 0.5174999999999995159 ) ) ;
#6734 = AXIS2_PLACEMENT_3D ( 'NONE', #11619, #12281, #4031 ) ;
#6735 = DIRECTION ( 'NONE',  ( -1.000000000000000000, -0.000000000000000000, -0.000000000000000000 ) ) ;
#6736 = CIRCLE ( 'NONE', #11361, 0.4070000000000025264 ) ;
#6737 = CARTESIAN_POINT ( 'NONE',  ( 2.280218097288460033, 0.5641718375784713357, -0.4677935297007478344 ) ) ;
#6738 = CARTESIAN_POINT ( 'NONE',  ( 0.9672769954795883418, -0.4829975555521405228, -0.4081482409675000200 ) ) ;
#6739 = ORIENTED_EDGE ( 'NONE', *, *, #14059, .F. ) ;
#6740 = CARTESIAN_POINT ( 'NONE',  ( 3.873439288382781065, 3.137999999999999901, 6.065921084684207584E-32 ) ) ;
#6741 = CARTESIAN_POINT ( 'NONE',  ( 3.652468232434641138, 1.936298606780756382, 0.4501807712518157145 ) ) ;
#6742 = CARTESIAN_POINT ( 'NONE',  ( 2.591520038054473840, 0.4049457270506677808, -0.4033906250602100618 ) ) ;
#6743 = EDGE_CURVE ( 'NONE', #13527, #4018, #8790, .T. ) ;
#6744 = AXIS2_PLACEMENT_3D ( 'NONE', #11739, #5923, #10581 ) ;
#6745 = CARTESIAN_POINT ( 'NONE',  ( 0.000000000000000000, 4.529999999999999361, 0.000000000000000000 ) ) ;
#6747 = EDGE_LOOP ( 'NONE', ( #13514, #11819, #189, #7058 ) ) ;
#6746 = DIRECTION ( 'NONE',  ( -0.000000000000000000, -1.000000000000000000, -0.000000000000000000 ) ) ;
#6748 = ORIENTED_EDGE ( 'NONE', *, *, #13237, .T. ) ;
#6749 = CIRCLE ( 'NONE', #8954, 0.06999999999999836908 ) ;
#6750 = AXIS2_PLACEMENT_3D ( 'NONE', #11974, #10977, #3942 ) ;
#6751 = DIRECTION ( 'NONE',  ( 1.000000000000000000, 0.000000000000000000, 0.000000000000000000 ) ) ;
#6752 = EDGE_LOOP ( 'NONE', ( #13215, #2206, #13012, #13717 ) ) ;
#6753 = FACE_OUTER_BOUND ( 'NONE', #4751, .T. ) ;
#6754 = EDGE_CURVE ( 'NONE', #5546, #5835, #12550, .T. ) ;
#6755 = DIRECTION ( 'NONE',  ( 0.000000000000000000, 0.000000000000000000, -1.000000000000000000 ) ) ;
#6756 = AXIS2_PLACEMENT_3D ( 'NONE', #14921, #5447, #10114 ) ;
#6757 = CARTESIAN_POINT ( 'NONE',  ( 0.7073825753665241578, -0.4455853224013471836, -0.4167523536742555601 ) ) ;
#6758 = DIRECTION ( 'NONE',  ( -1.000000000000000000, -0.000000000000000000, 0.000000000000000000 ) ) ;
#6759 = CARTESIAN_POINT ( 'NONE',  ( 0.7513246802501661881, 0.000000000000000000, -0.4293820849162031661 ) ) ;
#6760 = VECTOR ( 'NONE', #10514, 39.37007874015748143 ) ;
#6761 = ORIENTED_EDGE ( 'NONE', *, *, #14209, .F. ) ;
#6762 = CARTESIAN_POINT ( 'NONE',  ( 0.000000000000000000, 0.1749999999999999889, -0.8000000000000000444 ) ) ;
#6763 = FACE_OUTER_BOUND ( 'NONE', #12239, .T. ) ;
#6764 = DIRECTION ( 'NONE',  ( -0.7071067811865350272, 0.7071067811865600072, 0.000000000000000000 ) ) ;
#6765 = ORIENTED_EDGE ( 'NONE', *, *, #15121, .F. ) ;
#6766 = DIRECTION ( 'NONE',  ( -1.000000000000000000, -0.000000000000000000, -0.000000000000000000 ) ) ;
#6767 = DIRECTION ( 'NONE',  ( 1.000000000000000000, 0.000000000000000000, 0.000000000000000000 ) ) ;
#6768 = ORIENTED_EDGE ( 'NONE', *, *, #10065, .T. ) ;
#6769 = LINE ( 'NONE', #13706, #14272 ) ;
#6770 = CARTESIAN_POINT ( 'NONE',  ( 0.6844575745811062317, -0.4385969160104463138, -0.4560057122457037981 ) ) ;
#6771 = EDGE_CURVE ( 'NONE', #10875, #1362, #3903, .T. ) ;
#6772 = AXIS2_PLACEMENT_3D ( 'NONE', #949, #6703, #5560 ) ;
#6773 = PRODUCT_RELATED_PRODUCT_CATEGORY ( 'part', '', ( #6544 ) ) ;
#6774 = CARTESIAN_POINT ( 'NONE',  ( 0.9618941676350062364, -0.4364129403843365895, -0.4539147763481607978 ) ) ;
#6775 = CARTESIAN_POINT ( 'NONE',  ( 3.437087787517782100, 2.053741209332538453, 0.2425028344550888282 ) ) ;
#6776 = AXIS2_PLACEMENT_3D ( 'NONE', #2876, #10919, #7337 ) ;
#6777 = EDGE_LOOP ( 'NONE', ( #8942, #14675, #1732, #14223 ) ) ;
#6778 =( BOUNDED_SURFACE ( )  B_SPLINE_SURFACE ( 3, 2, ( 
 ( #1656, #6349, #8421 ),
 ( #13136, #7348, #421 ),
 ( #8495, #2602, #1439 ),
 ( #8569, #11001, #6128 ),
 ( #10786, #273, #4976 ),
 ( #9642, #14289, #5187 ),
 ( #2677, #12002, #6193 ),
 ( #10852, #2029, #14743 ),
 ( #6572, #7709, #6714 ),
 ( #6643, #10161, #8705 ),
 ( #565, #1799, #2967 ),
 ( #6412, #1725, #7790 ),
 ( #11068, #7861, #4198 ),
 ( #3197, #7628, #5262 ),
 ( #10017, #12288, #4345 ),
 ( #12368, #12510, #11297 ),
 ( #6491, #11228, #2893 ),
 ( #4270, #724, #5422 ) ),
 .UNSPECIFIED., .F., .F., .F. ) 
 B_SPLINE_SURFACE_WITH_KNOTS ( ( 4, 2, 2, 2, 2, 2, 2, 2, 4 ),
 ( 3, 3 ),
 ( 1.626303258728256651E-18, 0.0007909791536113771216, 0.001581958307222752725, 0.002372937460834128112, 0.003163916614445503716, 0.003954895768056879320, 0.004745874921668254490, 0.005536854075279630527, 0.006327833228891005697 ),
 ( 0.000000000000000000, 1.000000000000000000 ),
 .UNSPECIFIED. ) 
 GEOMETRIC_REPRESENTATION_ITEM ( )  RATIONAL_B_SPLINE_SURFACE ( (
 ( 1.000000000000000000, 0.7071067811865485719, 1.000000000000000000),
 ( 1.000000000000000000, 0.7223000759815237926, 1.000000000000000000),
 ( 1.000000000000000000, 0.7432471854318939419, 1.000000000000000000),
 ( 1.000000000000000000, 0.7877081205363730687, 1.000000000000000000),
 ( 1.000000000000000000, 0.8105118531247716973, 1.000000000000000000),
 ( 1.000000000000000000, 0.8506981922268006535, 1.000000000000000000),
 ( 1.000000000000000000, 0.8680068107956325774, 1.000000000000000000),
 ( 1.000000000000000000, 0.8928257656524388741, 1.000000000000000000),
 ( 1.000000000000000000, 0.9004767918862143228, 1.000000000000000000),
 ( 1.000000000000000000, 0.9031067434151224260, 1.000000000000000000),
 ( 1.000000000000000000, 0.8981097434906895050, 1.000000000000000000),
 ( 1.000000000000000000, 0.8774757945656930236, 1.000000000000000000),
 ( 1.000000000000000000, 0.8617372505914389080, 1.000000000000000000),
 ( 1.000000000000000000, 0.8241150794756328946, 1.000000000000000000),
 ( 1.000000000000000000, 0.8017387543657485960, 1.000000000000000000),
 ( 1.000000000000000000, 0.7573703026982906428, 1.000000000000000000),
 ( 1.000000000000000000, 0.7351444931784540948, 1.000000000000000000),
 ( 1.000000000000000000, 0.7173416231802117737, 1.000000000000000000) ) ) 
 REPRESENTATION_ITEM ( '' )  SURFACE ( )  );
#6779 = EDGE_LOOP ( 'NONE', ( #4427, #107, #13916, #6739 ) ) ;
#6780 = CIRCLE ( 'NONE', #7509, 3.000000000000000444 ) ;
#6781 = EDGE_LOOP ( 'NONE', ( #8365, #2439, #2351, #13438 ) ) ;
#6782 = CARTESIAN_POINT ( 'NONE',  ( -0.4349147617188193760, 1.559103846021574480, -0.008611041693309614414 ) ) ;
#6783 = ORIENTED_EDGE ( 'NONE', *, *, #5978, .T. ) ;
#6784 = DIRECTION ( 'NONE',  ( 0.000000000000000000, 1.000000000000000000, 0.000000000000000000 ) ) ;
#6785 = DIRECTION ( 'NONE',  ( -0.9999002670844989726, 0.000000000000000000, 0.01412288512831212997 ) ) ;
#6786 = CARTESIAN_POINT ( 'NONE',  ( 2.980731298636167370, 3.137999999999999901, 0.3249191361593797844 ) ) ;
#6787 = CARTESIAN_POINT ( 'NONE',  ( 2.230477600021715912, 0.4287871555018996084, 0.4684960790957384824 ) ) ;
#6788 = ORIENTED_EDGE ( 'NONE', *, *, #6624, .T. ) ;
#6789 = PRODUCT_RELATED_PRODUCT_CATEGORY ( 'part', '', ( #8859 ) ) ;
#6790 = CARTESIAN_POINT ( 'NONE',  ( 3.232037046709189898, 2.470280355568556185, -0.3878822227790326704 ) ) ;
#6791 = VECTOR ( 'NONE', #9085, 39.37007874015748143 ) ;
#6792 = CARTESIAN_POINT ( 'NONE',  ( 0.7073375012242669735, 0.002604401085336686614, -0.4168187156544767569 ) ) ;
#6793 = CARTESIAN_POINT ( 'NONE',  ( 3.874999999999999556, 3.105999999999998984, 1.320000000000000062 ) ) ;
#6794 = CIRCLE ( 'NONE', #14118, 0.2499999999999999167 ) ;
#6795 = DIRECTION ( 'NONE',  ( 0.000000000000000000, 0.000000000000000000, 1.000000000000000000 ) ) ;
#6796 = CARTESIAN_POINT ( 'NONE',  ( 4.586165101391412868, 1.802583718471729268, -0.2454321292609802641 ) ) ;
#6798 = EDGE_LOOP ( 'NONE', ( #2860, #6292, #5539, #9424 ) ) ;
#6797 = DIRECTION ( 'NONE',  ( -1.000000000000000000, -0.000000000000000000, -0.000000000000000000 ) ) ;
#6799 = CIRCLE ( 'NONE', #8748, 0.2625000000000000111 ) ;
#6800 = ORIENTED_EDGE ( 'NONE', *, *, #3989, .T. ) ;
#6802 = ORIENTED_EDGE ( 'NONE', *, *, #3291, .F. ) ;
#6801 = DIRECTION ( 'NONE',  ( -1.000000000000000000, -0.000000000000000000, -0.000000000000000000 ) ) ;
#6803 = ORIENTED_EDGE ( 'NONE', *, *, #8840, .F. ) ;
#6804 = EDGE_CURVE ( 'NONE', #4100, #803, #7793, .T. ) ;
#6805 = EDGE_CURVE ( 'NONE', #9590, #7408, #960, .T. ) ;
#6806 = DIRECTION ( 'NONE',  ( 1.000000000000000000, 0.000000000000000000, 0.000000000000000000 ) ) ;
#6807 =( NAMED_UNIT ( * ) SI_UNIT ( $, .STERADIAN. ) SOLID_ANGLE_UNIT ( ) );
#6808 = LINE ( 'NONE', #808, #581 ) ;
#6809 =( BOUNDED_CURVE ( )  B_SPLINE_CURVE ( 3, ( #11195, #12637, #8990, #927 ),
 .UNSPECIFIED., .F., .F. ) 
 B_SPLINE_CURVE_WITH_KNOTS ( ( 4, 4 ),
 ( 0.7853981633974467247, 1.570796326794896780 ),
 .UNSPECIFIED. ) 
 CURVE ( )  GEOMETRIC_REPRESENTATION_ITEM ( )  RATIONAL_B_SPLINE_CURVE ( ( 1.000000000000000000, 0.9492530216741910110, 0.9492530216741910110, 1.000000000000000000 ) ) 
 REPRESENTATION_ITEM ( '' )  );
#6810 = EDGE_LOOP ( 'NONE', ( #13933, #13838, #11305, #3398, #759, #3911, #3388, #230, #13937, #2668, #14717, #14945 ) ) ;
#6811 = ADVANCED_FACE ( 'NONE', ( #8864 ), #9023, .T. ) ;
#6812 = DIRECTION ( 'NONE',  ( -0.000000000000000000, -1.000000000000000000, -0.000000000000000000 ) ) ;
#6813 = CARTESIAN_POINT ( 'NONE',  ( 2.156999999999999140, -1.679378605318041950, 1.416878605318058870 ) ) ;
#6814 = AXIS2_PLACEMENT_3D ( 'NONE', #13451, #7960, #5594 ) ;
#6815 = VECTOR ( 'NONE', #1872, 39.37007874015748143 ) ;
#6816 = DIRECTION ( 'NONE',  ( 0.000000000000000000, 0.000000000000000000, 1.000000000000000000 ) ) ;
#6817 = CARTESIAN_POINT ( 'NONE',  ( 2.124999999999999556, -2.399999999999999911, 0.6999999999999997335 ) ) ;
#6818 = EDGE_CURVE ( 'NONE', #12391, #14596, #8661, .T. ) ;
#6819 = VECTOR ( 'NONE', #13293, 39.37007874015748143 ) ;
#6820 = EDGE_CURVE ( 'NONE', #1866, #14657, #7653, .T. ) ;
#6821 = CARTESIAN_POINT ( 'NONE',  ( 0.09500000000000168032, 3.673940397442060361E-16, -3.000000000000000444 ) ) ;
#6822 = DIRECTION ( 'NONE',  ( -1.000000000000000000, -0.000000000000000000, -0.000000000000000000 ) ) ;
#6823 = VERTEX_POINT ( 'NONE', #10311 ) ;
#6824 = DIRECTION ( 'NONE',  ( -1.000000000000000000, -0.000000000000000000, -0.000000000000000000 ) ) ;
#6825 = CONICAL_SURFACE ( 'NONE', #14611, 1.932031071636253650, 0.2617993877991429685 ) ;
#6826 = CARTESIAN_POINT ( 'NONE',  ( 3.402054984780856550, 0.9867414601700450483, -0.1630887597480132623 ) ) ;
#6827 = VECTOR ( 'NONE', #1459, 39.37007874015748143 ) ;
#6828 = CARTESIAN_POINT ( 'NONE',  ( 4.111306219097818904, 1.727883204818585483, -0.7590129541647976374 ) ) ;
#6829 = CIRCLE ( 'NONE', #1417, 0.4070000000000046914 ) ;
#6830 = FACE_OUTER_BOUND ( 'NONE', #12043, .T. ) ;
#6832 = ORIENTED_EDGE ( 'NONE', *, *, #8401, .F. ) ;
#6831 = CARTESIAN_POINT ( 'NONE',  ( 2.124999999999999556, 2.400000000000010569, 0.6999999999999612088 ) ) ;
#6833 = ORIENTED_EDGE ( 'NONE', *, *, #8664, .F. ) ;
#6834 = VECTOR ( 'NONE', #2813, 39.37007874015748143 ) ;
#6835 = DIRECTION ( 'NONE',  ( -0.9999002670844991947, 0.000000000000000000, -0.01412288512831586830 ) ) ;
#6836 = AXIS2_PLACEMENT_3D ( 'NONE', #10685, #10534, #9619 ) ;
#6837 = CARTESIAN_POINT ( 'NONE',  ( 2.414213562373087374, 0.1427864376268978830, 0.4064941968476759038 ) ) ;
#6838 = CARTESIAN_POINT ( 'NONE',  ( 2.738128344600899933, 0.4573395005112720901, -0.4018406495283275981 ) ) ;
#6839 = DIRECTION ( 'NONE',  ( 0.000000000000000000, 0.000000000000000000, 1.000000000000000000 ) ) ;
#6840 = CARTESIAN_POINT ( 'NONE',  ( 2.124999999999999556, -1.679378605318041950, 1.384878605318059064 ) ) ;
#6841 = CARTESIAN_POINT ( 'NONE',  ( 2.774999999999999911, 1.679378605318059048, 1.973878605318040158 ) ) ;
#6842 = ADVANCED_FACE ( 'NONE', ( #5652 ), #14674, .T. ) ;
#6843 = CIRCLE ( 'NONE', #11965, 0.4849999999999995981 ) ;
#6844 = ORIENTED_EDGE ( 'NONE', *, *, #10917, .T. ) ;
#6845 = DIRECTION ( 'NONE',  ( 0.1062487806292201492, -7.256387954780240841E-16, 0.9943395781194692695 ) ) ;
#6846 = CYLINDRICAL_SURFACE ( 'NONE', #1759, 0.3750000000000004996 ) ;
#6847 = VERTEX_POINT ( 'NONE', #6718 ) ;
#6848 = ADVANCED_FACE ( 'NONE', ( #5497, #14746, #4497, #7630 ), #12291, .T. ) ;
#6849 = CARTESIAN_POINT ( 'NONE',  ( 4.769268701363833074, 2.750000000000000000, -0.3249191361593796734 ) ) ;
#6850 = ORIENTED_EDGE ( 'NONE', *, *, #8015, .T. ) ;
#6851 = DIRECTION ( 'NONE',  ( 0.000000000000000000, 0.000000000000000000, 1.000000000000000000 ) ) ;
#6852 = ORIENTED_EDGE ( 'NONE', *, *, #8587, .T. ) ;
#6853 = DIRECTION ( 'NONE',  ( 0.000000000000000000, 0.000000000000000000, -1.000000000000000000 ) ) ;
#6854 = DIRECTION ( 'NONE',  ( 0.000000000000000000, -1.000000000000000000, -0.000000000000000000 ) ) ;
#6855 = VECTOR ( 'NONE', #458, 39.37007874015748143 ) ;
#6856 = CARTESIAN_POINT ( 'NONE',  ( 0.8803859122989420305, -0.4304857796780524049, -0.4642829517559106112 ) ) ;
#6857 = CARTESIAN_POINT ( 'NONE',  ( 3.490426473332387758, 2.028536269912275536, 0.3203772365046669846 ) ) ;
#6858 = APPLICATION_CONTEXT ( 'automotive_design' ) ;
#6859 = DIRECTION ( 'NONE',  ( 0.000000000000000000, 0.000000000000000000, -1.000000000000000000 ) ) ;
#6860 = DIRECTION ( 'NONE',  ( -0.000000000000000000, -1.000000000000000000, -0.000000000000000000 ) ) ;
#6861 = EDGE_CURVE ( 'NONE', #282, #7304, #12523, .T. ) ;
#6862 = EDGE_CURVE ( 'NONE', #3928, #11740, #15099, .T. ) ;
#6863 = ORIENTED_EDGE ( 'NONE', *, *, #14059, .T. ) ;
#6864 = VERTEX_POINT ( 'NONE', #728 ) ;
#6865 = LINE ( 'NONE', #9859, #6506 ) ;
#6866 = ORIENTED_EDGE ( 'NONE', *, *, #10727, .T. ) ;
#6867 = DIRECTION ( 'NONE',  ( 0.7071067811865474617, 0.000000000000000000, -0.7071067811865474617 ) ) ;
#6868 = FACE_OUTER_BOUND ( 'NONE', #1809, .T. ) ;
#6869 = DIRECTION ( 'NONE',  ( 0.000000000000000000, -1.000000000000000000, -0.000000000000000000 ) ) ;
#6870 = FACE_OUTER_BOUND ( 'NONE', #2023, .T. ) ;
#6871 = ORIENTED_EDGE ( 'NONE', *, *, #1182, .T. ) ;
#6872 = AXIS2_PLACEMENT_3D ( 'NONE', #8399, #13037, #3657 ) ;
#6873 = DIRECTION ( 'NONE',  ( 0.000000000000000000, 0.000000000000000000, 1.000000000000000000 ) ) ;
#6874 = CARTESIAN_POINT ( 'NONE',  ( 0.7013557507355751008, -0.03211000548724558118, -0.4833783981792019180 ) ) ;
#6875 = DIRECTION ( 'NONE',  ( 0.03489949670248613384, -0.9993908270190963172, 0.000000000000000000 ) ) ;
#6876 = CARTESIAN_POINT ( 'NONE',  ( 3.874999999999999556, 3.137999999999999901, -1.320000000000000062 ) ) ;
#6877 = VECTOR ( 'NONE', #9852, 39.37007874015748143 ) ;
#6878 = EDGE_CURVE ( 'NONE', #14332, #3499, #540, .T. ) ;
#6879 = CARTESIAN_POINT ( 'NONE',  ( 4.606274573907592540, 1.806393012917786534, -0.1768982737102013092 ) ) ;
#6880 = EDGE_LOOP ( 'NONE', ( #10711, #6844, #10134, #14513 ) ) ;
#6882 = VERTEX_POINT ( 'NONE', #10163 ) ;
#6881 = CARTESIAN_POINT ( 'NONE',  ( 3.426491571325181340, 3.360000000000016751, 0.9799999999999461364 ) ) ;
#6883 = ORIENTED_EDGE ( 'NONE', *, *, #5649, .F. ) ;
#6885 = EDGE_LOOP ( 'NONE', ( #11993, #13468 ) ) ;
#6884 = LINE ( 'NONE', #4502, #12855 ) ;
#6886 = EDGE_LOOP ( 'NONE', ( #6990, #12224, #12751, #11336 ) ) ;
#6887 = CARTESIAN_POINT ( 'NONE',  ( 0.1250000000000009992, 0.000000000000000000, 1.000000000000000000 ) ) ;
#6888 = CARTESIAN_POINT ( 'NONE',  ( -0.4124999999999999223, 0.1749999999999999889, -0.4124999999999999778 ) ) ;
#6889 = VERTEX_POINT ( 'NONE', #14899 ) ;
#6890 = DIRECTION ( 'NONE',  ( -0.01412288512831213171, 3.675428035873182550E-19, -0.9999002670844991947 ) ) ;
#6891 = CARTESIAN_POINT ( 'NONE',  ( 0.6678556410416571776, -0.4638629127466907254, -0.4666787114416890425 ) ) ;
#6892 = CARTESIAN_POINT ( 'NONE',  ( 2.806999999999999496, -1.679378605318041950, 1.941878605318059003 ) ) ;
#6893 =( GEOMETRIC_REPRESENTATION_CONTEXT ( 3 ) GLOBAL_UNCERTAINTY_ASSIGNED_CONTEXT ( ( #3563 ) ) GLOBAL_UNIT_ASSIGNED_CONTEXT ( ( #4167, #7674, #5389 ) ) REPRESENTATION_CONTEXT ( 'NONE', 'WORKASPACE' ) );
#6894 = DIRECTION ( 'NONE',  ( 1.000000000000000000, 0.000000000000000000, 0.000000000000000000 ) ) ;
#6895 = ADVANCED_FACE ( 'NONE', ( #7938 ), #4425, .F. ) ;
#6896 = DIRECTION ( 'NONE',  ( -1.000000000000000000, 0.000000000000000000, 0.000000000000000000 ) ) ;
#6897 = CARTESIAN_POINT ( 'NONE',  ( 2.650000000000001688, 0.000000000000000000, 0.000000000000000000 ) ) ;
#6898 = ADVANCED_FACE ( 'NONE', ( #7183 ), #8179, .T. ) ;
#6899 = CARTESIAN_POINT ( 'NONE',  ( 2.124999999999999556, 1.679378605318042395, -1.679378605318058604 ) ) ;
#6900 = LINE ( 'NONE', #9346, #684 ) ;
#6901 = DIRECTION ( 'NONE',  ( 0.000000000000000000, 0.000000000000000000, 1.000000000000000000 ) ) ;
#6902 = CIRCLE ( 'NONE', #8842, 0.2220000000000021678 ) ;
#6903 = CARTESIAN_POINT ( 'NONE',  ( 3.394491571325183088, 1.679378605318059048, 1.679378605318041506 ) ) ;
#6905 = VERTEX_POINT ( 'NONE', #4891 ) ;
#6904 = FACE_OUTER_BOUND ( 'NONE', #14556, .T. ) ;
#6906 = EDGE_LOOP ( 'NONE', ( #10580, #3298, #5301, #2738 ) ) ;
#6907 = EDGE_CURVE ( 'NONE', #5546, #4834, #5819, .T. ) ;
#6908 = DIRECTION ( 'NONE',  ( 0.000000000000000000, -1.000000000000000000, 0.000000000000000000 ) ) ;
#6909 = ORIENTED_EDGE ( 'NONE', *, *, #11483, .F. ) ;
#6910 = DIRECTION ( 'NONE',  ( -1.000000000000000000, -0.000000000000000000, -0.000000000000000000 ) ) ;
#6911 = CARTESIAN_POINT ( 'NONE',  ( 6.176491571325181340, 0.000000000000000000, 0.000000000000000000 ) ) ;
#6912 = DIRECTION ( 'NONE',  ( -1.000000000000000000, -0.000000000000000000, -0.000000000000000000 ) ) ;
#6913 = EDGE_CURVE ( 'NONE', #11132, #8878, #8631, .T. ) ;
#6914 = DIRECTION ( 'NONE',  ( 1.000000000000000000, 0.000000000000000000, 0.000000000000000000 ) ) ;
#6915 = ORIENTED_EDGE ( 'NONE', *, *, #422, .F. ) ;
#6916 = EDGE_CURVE ( 'NONE', #11155, #6614, #4724, .T. ) ;
#6917 = CARTESIAN_POINT ( 'NONE',  ( 0.6782634401674774161, -0.4298497817134653287, 0.4690018541713363853 ) ) ;
#6918 = CARTESIAN_POINT ( 'NONE',  ( 3.426491571325181340, -2.359999999999979892, 1.575000000000016387 ) ) ;
#6919 = VERTEX_POINT ( 'NONE', #11610 ) ;
#6920 = DIRECTION ( 'NONE',  ( -0.9993908270190959842, -0.03489949670249406499, 0.000000000000000000 ) ) ;
#6921 = ORIENTED_EDGE ( 'NONE', *, *, #1765, .T. ) ;
#6922 = AXIS2_PLACEMENT_3D ( 'NONE', #2841, #7582, #5596 ) ;
#6923 = DIRECTION ( 'NONE',  ( 1.000000000000000000, 0.000000000000000000, 0.000000000000000000 ) ) ;
#6924 = ORIENTED_EDGE ( 'NONE', *, *, #1694, .T. ) ;
#6925 = EDGE_CURVE ( 'NONE', #8503, #13119, #4477, .T. ) ;
#6926 = DIRECTION ( 'NONE',  ( -0.9659258262890698665, 0.000000000000000000, 0.2588190451025147443 ) ) ;
#6927 = CARTESIAN_POINT ( 'NONE',  ( 0.9703582086188188294, -0.4381469060595838960, -0.4503728430570826391 ) ) ;
#6928 = ADVANCED_FACE ( 'NONE', ( #13963 ), #5802, .F. ) ;
#6929 = DIRECTION ( 'NONE',  ( 0.7071067811865421326, 0.000000000000000000, -0.7071067811865527908 ) ) ;
#6930 = DIRECTION ( 'NONE',  ( 0.000000000000000000, 1.000000000000000000, 0.000000000000000000 ) ) ;
#6931 = VECTOR ( 'NONE', #5950, 39.37007874015748143 ) ;
#6932 = CARTESIAN_POINT ( 'NONE',  ( 3.741597707132858108, 1.905344493321387889, -0.7379504897677242603 ) ) ;
#6933 = EDGE_LOOP ( 'NONE', ( #1478, #3526, #1424, #5908 ) ) ;
#6934 = VERTEX_POINT ( 'NONE', #7117 ) ;
#6935 = ADVANCED_FACE ( 'NONE', ( #10692 ), #14043, .F. ) ;
#6936 = VECTOR ( 'NONE', #2551, 39.37007874015748143 ) ;
#6937 = CARTESIAN_POINT ( 'NONE',  ( 1.007186596135057011, -0.4429912711639673040, -0.4173593519128859231 ) ) ;
#6938 = ORIENTED_EDGE ( 'NONE', *, *, #8804, .T. ) ;
#6939 = CARTESIAN_POINT ( 'NONE',  ( 0.2936244729112413299, 1.600827805288693062, -0.2533330005241143934 ) ) ;
#6940 = CARTESIAN_POINT ( 'NONE',  ( 2.774999999999999911, -2.399999999999999911, 0.6999999999999997335 ) ) ;
#6941 = FACE_BOUND ( 'NONE', #1039, .T. ) ;
#6942 = CARTESIAN_POINT ( 'NONE',  ( 2.774999999999999911, 1.575000000000016165, 2.359999999999999876 ) ) ;
#6943 = VERTEX_POINT ( 'NONE', #3583 ) ;
#6944 = DIRECTION ( 'NONE',  ( 0.000000000000000000, 0.000000000000000000, -1.000000000000000000 ) ) ;
#6945 = ADVANCED_FACE ( 'NONE', ( #5885 ), #2528, .F. ) ;
#6946 = CARTESIAN_POINT ( 'NONE',  ( 0.7134904538003046248, -1.707404996040164512E-17, -0.4077598229816902231 ) ) ;
#6947 = AXIS2_PLACEMENT_3D ( 'NONE', #2288, #9781, #8633 ) ;
#6948 = CARTESIAN_POINT ( 'NONE',  ( 2.633946444925666874, 0.3625193201794746356, -0.4033906250602100618 ) ) ;
#6949 = AXIS2_PLACEMENT_3D ( 'NONE', #10336, #6835, #2225 ) ;
#6950 = PLANE ( 'NONE',  #771 ) ;
#6951 = CARTESIAN_POINT ( 'NONE',  ( 4.685776054466175289, 1.733272791389190548, 0.03942178684877539058 ) ) ;
#6953 = VERTEX_POINT ( 'NONE', #8263 ) ;
#6952 = CARTESIAN_POINT ( 'NONE',  ( 0.2845281682845477444, 1.599152118624413976, 0.2690882622986748296 ) ) ;
#6954 = ORIENTED_EDGE ( 'NONE', *, *, #3518, .F. ) ;
#6955 = CIRCLE ( 'NONE', #2553, 0.06000000000000008105 ) ;
#6957 = ORIENTED_EDGE ( 'NONE', *, *, #12871, .F. ) ;
#6956 = CARTESIAN_POINT ( 'NONE',  ( 2.774999999999999911, 0.000000000000000000, 1.039370078740158965 ) ) ;
#6958 = ORIENTED_EDGE ( 'NONE', *, *, #4785, .T. ) ;
#6959 = DIRECTION ( 'NONE',  ( 0.000000000000000000, 1.000000000000000000, 0.000000000000000000 ) ) ;
#6960 = SHAPE_REPRESENTATION_RELATIONSHIP ( 'NONE' , 'NONE' ,  #8297, #14952 ) ;
#6961 = DIRECTION ( 'NONE',  ( 0.000000000000000000, 0.000000000000000000, -1.000000000000000000 ) ) ;
#6962 = ORIENTED_EDGE ( 'NONE', *, *, #78, .T. ) ;
#6963 = DIRECTION ( 'NONE',  ( -1.000000000000000000, -0.000000000000000000, -0.000000000000000000 ) ) ;
#6964 = CARTESIAN_POINT ( 'NONE',  ( 0.6735138268600964206, -0.4714177217989499180, -0.4544009417003763152 ) ) ;
#6965 = EDGE_CURVE ( 'NONE', #8303, #11264, #10388, .T. ) ;
#6966 = DIRECTION ( 'NONE',  ( 0.000000000000000000, 0.000000000000000000, -1.000000000000000000 ) ) ;
#6967 = DIRECTION ( 'NONE',  ( 0.000000000000000000, 0.7071067811865491270, 0.7071067811865459074 ) ) ;
#6968 = AXIS2_PLACEMENT_3D ( 'NONE', #3761, #3612, #8433 ) ;
#6969 = DIRECTION ( 'NONE',  ( 0.01412288512831213171, -3.675428035873182550E-19, 0.9999002670844991947 ) ) ;
#6970 = CIRCLE ( 'NONE', #6477, 0.9999999999999998890 ) ;
#6971 = FACE_OUTER_BOUND ( 'NONE', #5812, .T. ) ;
#6972 = FACE_BOUND ( 'NONE', #4241, .T. ) ;
#6973 = CARTESIAN_POINT ( 'NONE',  ( 3.510666870471307988, 0.9394827552388973491, 0.3428102772992727143 ) ) ;
#6974 = CARTESIAN_POINT ( 'NONE',  ( 2.774999999999999911, -1.679378605318059048, -1.941878605318027251 ) ) ;
#6975 = ORIENTED_EDGE ( 'NONE', *, *, #13478, .F. ) ;
#6976 = DIRECTION ( 'NONE',  ( -0.000000000000000000, -1.000000000000000000, -0.000000000000000000 ) ) ;
#6978 = ORIENTED_EDGE ( 'NONE', *, *, #13518, .F. ) ;
#6977 = DIRECTION ( 'NONE',  ( -0.7071067811865429098, 8.659560562354987092E-17, -0.7071067811865521247 ) ) ;
#6979 = VERTEX_POINT ( 'NONE', #10613 ) ;
#6980 = AXIS2_PLACEMENT_3D ( 'NONE', #11307, #2121, #887 ) ;
#6981 = CARTESIAN_POINT ( 'NONE',  ( 0.3725000000000000533, 0.000000000000000000, -0.4124999999999999778 ) ) ;
#6982 = ORIENTED_EDGE ( 'NONE', *, *, #9050, .F. ) ;
#6983 = CARTESIAN_POINT ( 'NONE',  ( 0.8999999999999998002, 0.000000000000000000, -0.3799999999999999489 ) ) ;
#6984 = VECTOR ( 'NONE', #14248, 39.37007874015748143 ) ;
#6985 = AXIS2_PLACEMENT_3D ( 'NONE', #11262, #3230, #12706 ) ;
#6986 = B_SPLINE_CURVE_WITH_KNOTS ( 'NONE', 3,
 ( #2497, #9393, #4954, #7109, #9618, #11830, #11756, #8470, #1256, #178, #6021, #10684, #4882, #14259, #3795, #13112, #5943, #2648, #7327, #11980 ),
 .UNSPECIFIED., .F., .F.,
 ( 4, 2, 2, 2, 2, 2, 2, 2, 2, 4 ),
 ( 4.481635188367946092E-07, 0.003578814135748883529, 0.005367997121863906339, 0.007157180107978928715, 0.008051771601036455950, 0.008946363094093984919, 0.01073554608020907929, 0.01252472906632417539, 0.01341932055938169915, 0.01431391205243922465 ),
 .UNSPECIFIED. ) ;
#6987 = CARTESIAN_POINT ( 'NONE',  ( 2.414213562373090927, 0.1427864376269009083, 0.4064941968476758483 ) ) ;
#6988 = FACE_OUTER_BOUND ( 'NONE', #140, .T. ) ;
#6989 = CARTESIAN_POINT ( 'NONE',  ( 2.774999999999999911, 2.359999999999994547, -1.575000000000016831 ) ) ;
#6990 = ORIENTED_EDGE ( 'NONE', *, *, #4977, .T. ) ;
#6991 = CIRCLE ( 'NONE', #5031, 0.3750000000000004996 ) ;
#6992 = CARTESIAN_POINT ( 'NONE',  ( 0.6867276282385307296, -0.4820986824598040843, 0.4280639610650029403 ) ) ;
#6993 = CARTESIAN_POINT ( 'NONE',  ( 3.601417382415921686, 0.9969999999999999973, 0.4491325228472327624 ) ) ;
#6994 = CONICAL_SURFACE ( 'NONE', #3557, 0.2625000000000000111, 0.7853981633974452814 ) ;
#6995 = CARTESIAN_POINT ( 'NONE',  ( 3.426491571325181340, 1.575000000000000178, -2.360000000000018971 ) ) ;
#6996 = VECTOR ( 'NONE', #5520, 39.37007874015748143 ) ;
#6997 = ORIENTED_EDGE ( 'NONE', *, *, #13660, .T. ) ;
#6998 = CARTESIAN_POINT ( 'NONE',  ( 7.623651669702752511E-17, -0.6589999999999998082, 0.000000000000000000 ) ) ;
#6999 = ORIENTED_EDGE ( 'NONE', *, *, #532, .F. ) ;
#7000 = DIRECTION ( 'NONE',  ( -1.000000000000000000, -0.000000000000000000, -0.000000000000000000 ) ) ;
#7001 = DIRECTION ( 'NONE',  ( -1.000000000000000000, -0.000000000000000000, -0.000000000000000000 ) ) ;
#7002 = ORIENTED_EDGE ( 'NONE', *, *, #8228, .T. ) ;
#7003 = EDGE_CURVE ( 'NONE', #6726, #8646, #2279, .T. ) ;
#7004 = DIRECTION ( 'NONE',  ( 0.000000000000000000, 1.224646799147354933E-16, 1.000000000000000000 ) ) ;
#7005 = EDGE_CURVE ( 'NONE', #7063, #1193, #8158, .T. ) ;
#7006 = VECTOR ( 'NONE', #1662, 39.37007874015748143 ) ;
#7007 = ADVANCED_FACE ( 'NONE', ( #5307 ), #2659, .F. ) ;
#7008 = CARTESIAN_POINT ( 'NONE',  ( 2.321652452206756756, 0.05022532746056743852, -0.4077623363510139431 ) ) ;
#7009 = CIRCLE ( 'NONE', #4794, 0.2944999999999845519 ) ;
#7010 = DIRECTION ( 'NONE',  ( 0.000000000000000000, 0.000000000000000000, -1.000000000000000000 ) ) ;
#7011 = EDGE_CURVE ( 'NONE', #524, #937, #14243, .T. ) ;
#7012 = CARTESIAN_POINT ( 'NONE',  ( 3.426491571325181340, 1.679378605318042395, -1.941878605318058337 ) ) ;
#7013 = AXIS2_PLACEMENT_3D ( 'NONE', #4428, #9171, #13737 ) ;
#7014 = CARTESIAN_POINT ( 'NONE',  ( 3.612497800988201835, 1.962888430913071414, -0.7027605075283567260 ) ) ;
#7015 = ORIENTED_EDGE ( 'NONE', *, *, #8358, .T. ) ;
#7016 = ORIENTED_EDGE ( 'NONE', *, *, #12221, .F. ) ;
#7017 = CARTESIAN_POINT ( 'NONE',  ( 2.742999999999999883, -1.679378605318041950, 1.679378605318059048 ) ) ;
#7018 = ORIENTED_EDGE ( 'NONE', *, *, #14453, .F. ) ;
#7019 = CARTESIAN_POINT ( 'NONE',  ( -0.4108223460329263887, 5.750000000000000000, -0.2850000000000042499 ) ) ;
#7020 = CIRCLE ( 'NONE', #10914, 0.4849999999999995981 ) ;
#7021 = CARTESIAN_POINT ( 'NONE',  ( 0.8917602750860615934, -0.4611956585980242496, -0.4498705880430254322 ) ) ;
#7022 = DIRECTION ( 'NONE',  ( 0.000000000000000000, 0.000000000000000000, 1.000000000000000000 ) ) ;
#7023 = ORIENTED_EDGE ( 'NONE', *, *, #5430, .T. ) ;
#7024 = DIRECTION ( 'NONE',  ( 0.000000000000000000, 0.000000000000000000, -1.000000000000000000 ) ) ;
#7025 = VECTOR ( 'NONE', #4714, 39.37007874015748143 ) ;
#7026 = CARTESIAN_POINT ( 'NONE',  ( 1.001102354577344311, -0.4429645722769263716, -0.4282009803966606576 ) ) ;
#7027 = DIRECTION ( 'NONE',  ( -1.000000000000000000, -0.000000000000000000, -0.000000000000000000 ) ) ;
#7028 = CARTESIAN_POINT ( 'NONE',  ( 2.003951500898716542, -0.1834701832127828836, -0.4716956002697923478 ) ) ;
#7029 = VECTOR ( 'NONE', #4484, 39.37007874015748143 ) ;
#7030 = EDGE_CURVE ( 'NONE', #11461, #9235, #14983, .T. ) ;
#7031 = CARTESIAN_POINT ( 'NONE',  ( 0.000000000000000000, 1.159999999999999698, 0.000000000000000000 ) ) ;
#7032 = CARTESIAN_POINT ( 'NONE',  ( 4.487607086153403202, 1.787994762819255623, -0.4363467488208105372 ) ) ;
#7033 = VERTEX_POINT ( 'NONE', #14554 ) ;
#7035 = ORIENTED_EDGE ( 'NONE', *, *, #2588, .F. ) ;
#7034 = CARTESIAN_POINT ( 'NONE',  ( 0.4150198198414020156, 1.581125151349147773, 0.04307009183862406387 ) ) ;
#7036 = EDGE_CURVE ( 'NONE', #6615, #2564, #3734, .T. ) ;
#7037 = AXIS2_PLACEMENT_3D ( 'NONE', #14416, #14334, #9904 ) ;
#7038 = ORIENTED_EDGE ( 'NONE', *, *, #11494, .T. ) ;
#7040 = ORIENTED_EDGE ( 'NONE', *, *, #3166, .T. ) ;
#7039 = DIRECTION ( 'NONE',  ( 1.000000000000000000, 0.000000000000000000, 0.000000000000000000 ) ) ;
#7041 = ORIENTED_EDGE ( 'NONE', *, *, #1714, .T. ) ;
#7042 = CARTESIAN_POINT ( 'NONE',  ( -5.764454660286586870E-18, 0.1956296296296295978, 0.000000000000000000 ) ) ;
#7043 = ORIENTED_EDGE ( 'NONE', *, *, #4747, .T. ) ;
#7044 = DIRECTION ( 'NONE',  ( -1.000000000000000000, 0.000000000000000000, 0.000000000000000000 ) ) ;
#7045 = DIRECTION ( 'NONE',  ( -0.000000000000000000, -1.000000000000000000, -0.000000000000000000 ) ) ;
#7046 = CARTESIAN_POINT ( 'NONE',  ( 0.9749999999999999778, -0.6230000000000016636, -0.3750000000000000555 ) ) ;
#7047 = LINE ( 'NONE', #3286, #4737 ) ;
#7048 = CARTESIAN_POINT ( 'NONE',  ( 3.874999999999999556, 2.782000000000002693, 1.509999999999999787 ) ) ;
#7049 = CONICAL_SURFACE ( 'NONE', #4856, 1.039370078740158965, 0.7853981633974517207 ) ;
#7050 = DIRECTION ( 'NONE',  ( -1.000000000000000000, -0.000000000000000000, -0.000000000000000000 ) ) ;
#7051 = CYLINDRICAL_SURFACE ( 'NONE', #2149, 1.000000000000000222 ) ;
#7052 = CARTESIAN_POINT ( 'NONE',  ( 2.591947913870973785, 0.4045262297594673373, 0.4633905661882630755 ) ) ;
#7053 = VECTOR ( 'NONE', #4506, 39.37007874015748143 ) ;
#7054 = CARTESIAN_POINT ( 'NONE',  ( 3.944129661530210385, 1.761538328845252188, 0.7935532608319412207 ) ) ;
#7055 = EDGE_CURVE ( 'NONE', #12114, #3491, #13251, .T. ) ;
#7056 = ORIENTED_EDGE ( 'NONE', *, *, #5436, .F. ) ;
#7058 = ORIENTED_EDGE ( 'NONE', *, *, #722, .F. ) ;
#7057 = DIRECTION ( 'NONE',  ( 1.000000000000000000, 0.000000000000000000, 0.000000000000000000 ) ) ;
#7059 = ORIENTED_EDGE ( 'NONE', *, *, #14930, .F. ) ;
#7060 = B_SPLINE_CURVE_WITH_KNOTS ( 'NONE', 3,
 ( #8392, #6095, #10598, #247, #21, #12803, #9612, #12729, #6937, #2335 ),
 .UNSPECIFIED., .F., .F.,
 ( 4, 2, 2, 2, 4 ),
 ( 1.734723475976807094E-18, 0.0007067171527782007247, 0.001413434305556399715, 0.002120151458334598813, 0.002826868611112797695 ),
 .UNSPECIFIED. ) ;
#7061 = DIRECTION ( 'NONE',  ( -0.000000000000000000, 1.000000000000000000, -0.000000000000000000 ) ) ;
#7062 = DIRECTION ( 'NONE',  ( -1.000000000000000000, -1.365923996832131609E-16, 0.000000000000000000 ) ) ;
#7063 = VERTEX_POINT ( 'NONE', #12335 ) ;
#7064 = AXIS2_PLACEMENT_3D ( 'NONE', #11901, #4567, #13874 ) ;
#7065 = CARTESIAN_POINT ( 'NONE',  ( 0.000000000000000000, -1.002374524060224757E-18, 0.000000000000000000 ) ) ;
#7066 = CIRCLE ( 'NONE', #2649, 0.1900000000000000577 ) ;
#7067 = APPLICATION_CONTEXT ( 'automotive_design' ) ;
#7068 = DIRECTION ( 'NONE',  ( -0.000000000000000000, -0.000000000000000000, -1.000000000000000000 ) ) ;
#7069 = CIRCLE ( 'NONE', #10965, 1.494001693158433230 ) ;
#7070 = LINE ( 'NONE', #5758, #1903 ) ;
#7071 = CONICAL_SURFACE ( 'NONE', #8302, 0.2944999999999998175, 0.7853981633974520538 ) ;
#7072 = ORIENTED_EDGE ( 'NONE', *, *, #706, .F. ) ;
#7073 = AXIS2_PLACEMENT_3D ( 'NONE', #4926, #8225, #2623 ) ;
#7074 = CARTESIAN_POINT ( 'NONE',  ( 0.6583927779709454198, -0.3799506946983937650, 0.5137831800632561841 ) ) ;
#7075 = CARTESIAN_POINT ( 'NONE',  ( 6.787121492585022509, 0.000000000000000000, 0.000000000000000000 ) ) ;
#7076 = DIRECTION ( 'NONE',  ( 1.000000000000000000, 0.000000000000000000, 0.000000000000000000 ) ) ;
#7077 = ORIENTED_EDGE ( 'NONE', *, *, #12405, .F. ) ;
#7078 = VECTOR ( 'NONE', #8930, 39.37007874015748143 ) ;
#7079 = CARTESIAN_POINT ( 'NONE',  ( 3.874999999999999556, 3.137999999999999901, -1.542500000000001315 ) ) ;
#7080 = VECTOR ( 'NONE', #13346, 39.37007874015748143 ) ;
#7081 = DIRECTION ( 'NONE',  ( -1.000000000000000000, -0.000000000000000000, -0.000000000000000000 ) ) ;
#7082 = EDGE_CURVE ( 'NONE', #13550, #14571, #9979, .T. ) ;
#7083 = ORIENTED_EDGE ( 'NONE', *, *, #12895, .F. ) ;
#7084 = CARTESIAN_POINT ( 'NONE',  ( 1.375000000000000000, 0.000000000000000000, 0.000000000000000000 ) ) ;
#7085 = EDGE_LOOP ( 'NONE', ( #3910, #8344, #12743, #8425 ) ) ;
#7086 = CONICAL_SURFACE ( 'NONE', #13881, 0.3750000000000004996, 0.7853981633974376209 ) ;
#7087 = CARTESIAN_POINT ( 'NONE',  ( 3.874999999999999556, 3.567999999999999616, 1.320000000000000062 ) ) ;
#7088 = VECTOR ( 'NONE', #5939, 39.37007874015748854 ) ;
#7089 = CARTESIAN_POINT ( 'NONE',  ( 2.220468100499630726, -0.03283382702689773003, -0.4686374562075200090 ) ) ;
#7090 = AXIS2_PLACEMENT_3D ( 'NONE', #9142, #4550, #12720 ) ;
#7091 = CARTESIAN_POINT ( 'NONE',  ( 0.3724999999999997757, 0.2159999999999999698, -0.3725000000000000533 ) ) ;
#7092 = CARTESIAN_POINT ( 'NONE',  ( 0.4425000000000001155, 0.2159999999999999420, -0.8500000000000000888 ) ) ;
#7093 = EDGE_CURVE ( 'NONE', #14462, #15055, #7334, .T. ) ;
#7094 = ADVANCED_FACE ( 'NONE', ( #11270 ), #6456, .T. ) ;
#7095 = EDGE_CURVE ( 'NONE', #12193, #8971, #4081, .T. ) ;
#7096 = CARTESIAN_POINT ( 'NONE',  ( 3.651772946692535271, 1.855017273657071586, -0.7749448188891172595 ) ) ;
#7097 = VERTEX_POINT ( 'NONE', #13118 ) ;
#7098 = ORIENTED_EDGE ( 'NONE', *, *, #14271, .F. ) ;
#7099 = VECTOR ( 'NONE', #683, 39.37007874015748143 ) ;
#7100 = UNCERTAINTY_MEASURE_WITH_UNIT (LENGTH_MEASURE( 1.000000000000000082E-05 ), #2204, 'distance_accuracy_value', 'NONE');
#7101 = CARTESIAN_POINT ( 'NONE',  ( 2.774999999999999911, -0.6999999999999598765, 2.400000000000012346 ) ) ;
#7102 = ORIENTED_EDGE ( 'NONE', *, *, #9050, .T. ) ;
#7103 = DIRECTION ( 'NONE',  ( -1.000000000000000000, -2.130223169792495565E-16, 0.000000000000000000 ) ) ;
#7104 = DIRECTION ( 'NONE',  ( 0.000000000000000000, 1.000000000000000000, -0.000000000000000000 ) ) ;
#7105 = CARTESIAN_POINT ( 'NONE',  ( 0.000000000000000000, 0.000000000000000000, 0.000000000000000000 ) ) ;
#7106 = EDGE_CURVE ( 'NONE', #788, #331, #8477, .T. ) ;
#7107 = CARTESIAN_POINT ( 'NONE',  ( 0.7441595030246632714, -3.474002255126643149E-17, -0.4356261515797149597 ) ) ;
#7108 = ORIENTED_EDGE ( 'NONE', *, *, #14522, .F. ) ;
#7109 = CARTESIAN_POINT ( 'NONE',  ( 3.520930857593272290, 1.966513645793204201, -0.3538087319994585034 ) ) ;
#7110 = CARTESIAN_POINT ( 'NONE',  ( 1.250847373107698557, 9.390727478220904197E-17, 0.4823326642216427262 ) ) ;
#7111 = DIRECTION ( 'NONE',  ( 1.000000000000000000, 0.000000000000000000, 0.000000000000000000 ) ) ;
#7112 = AXIS2_PLACEMENT_3D ( 'NONE', #2673, #7345, #11923 ) ;
#7113 = EDGE_CURVE ( 'NONE', #1040, #6548, #13400, .T. ) ;
#7114 = DIRECTION ( 'NONE',  ( -0.000000000000000000, -1.000000000000000000, -0.000000000000000000 ) ) ;
#7115 = CARTESIAN_POINT ( 'NONE',  ( 4.626010065331895404, 1.749087012044151512, -0.03377502978455236560 ) ) ;
#7116 = ORIENTED_EDGE ( 'NONE', *, *, #8856, .T. ) ;
#7118 = ORIENTED_EDGE ( 'NONE', *, *, #4780, .T. ) ;
#7117 = CARTESIAN_POINT ( 'NONE',  ( -0.4124999999999999223, 0.000000000000000000, -0.3724999999999999978 ) ) ;
#7119 = ORIENTED_EDGE ( 'NONE', *, *, #885, .T. ) ;
#7120 = CARTESIAN_POINT ( 'NONE',  ( 0.09500000000000431710, 1.679378605318035733, -2.054378605318066153 ) ) ;
#7121 = ORIENTED_EDGE ( 'NONE', *, *, #3123, .F. ) ;
#7122 = LINE ( 'NONE', #11918, #14778 ) ;
#7123 = VERTEX_POINT ( 'NONE', #2937 ) ;
#7124 = CARTESIAN_POINT ( 'NONE',  ( 0.000000000000000000, 0.000000000000000000, 0.000000000000000000 ) ) ;
#7125 = DIRECTION ( 'NONE',  ( 1.000000000000000000, 0.000000000000000000, 0.000000000000000000 ) ) ;
#7126 = ADVANCED_FACE ( 'NONE', ( #13548 ), #10768, .T. ) ;
#7127 = FACE_OUTER_BOUND ( 'NONE', #11821, .T. ) ;
#7128 = DIRECTION ( 'NONE',  ( -1.000000000000000000, -0.000000000000000000, -0.000000000000000000 ) ) ;
#7129 = EDGE_CURVE ( 'NONE', #9822, #9131, #14000, .T. ) ;
#7130=STYLED_ITEM('',(#15206),#5553);
#7131 = CARTESIAN_POINT ( 'NONE',  ( 0.06299999999999994493, 0.000000000000000000, 0.000000000000000000 ) ) ;
#7132 = CARTESIAN_POINT ( 'NONE',  ( 2.774999999999999911, 3.360000000000000320, -0.9800000000000012035 ) ) ;
#7133 = CARTESIAN_POINT ( 'NONE',  ( 0.1007315414569005807, 0.1749999999999999889, -0.7936328852534507705 ) ) ;
#7134 = FACE_OUTER_BOUND ( 'NONE', #2199, .T. ) ;
#7135 = VERTEX_POINT ( 'NONE', #11910 ) ;
#7136 = DIRECTION ( 'NONE',  ( -1.000000000000000000, -0.000000000000000000, -0.000000000000000000 ) ) ;
#7138 = ORIENTED_EDGE ( 'NONE', *, *, #12678, .T. ) ;
#7137 = CARTESIAN_POINT ( 'NONE',  ( -0.6412116890856959239, -0.6590000000000000302, 0.000000000000000000 ) ) ;
#7139 = ORIENTED_EDGE ( 'NONE', *, *, #977, .T. ) ;
#7140 = DIRECTION ( 'NONE',  ( 0.000000000000000000, 1.000000000000000000, 0.000000000000000000 ) ) ;
#7141 = CARTESIAN_POINT ( 'NONE',  ( 0.8999999999999999112, -0.6230000000000016636, -0.3750000000000000555 ) ) ;
#7142 = CARTESIAN_POINT ( 'NONE',  ( 2.702105678819866963, 0.5048229836667779136, 0.4618346655533916989 ) ) ;
#7143 = EDGE_LOOP ( 'NONE', ( #7138, #4659 ) ) ;
#7144 = AXIS2_PLACEMENT_3D ( 'NONE', #3774, #13165, #4770 ) ;
#7145 = DIRECTION ( 'NONE',  ( 0.000000000000000000, 0.000000000000000000, 1.000000000000000000 ) ) ;
#7146 = ADVANCED_FACE ( 'NONE', ( #5033 ), #4244, .F. ) ;
#7147 = EDGE_CURVE ( 'NONE', #2489, #5710, #12373, .T. ) ;
#7148 = CARTESIAN_POINT ( 'NONE',  ( 6.826491571325181695, 3.673940397442060361E-16, -3.000000000000000444 ) ) ;
#7149 = CARTESIAN_POINT ( 'NONE',  ( 0.8852856429364857060, 0.000000000000000000, -0.2372115730956926294 ) ) ;
#7150 = EDGE_LOOP ( 'NONE', ( #8071, #1854, #12374, #13734 ) ) ;
#7151 = DIRECTION ( 'NONE',  ( 0.000000000000000000, 1.000000000000000000, -0.000000000000000000 ) ) ;
#7152 = CARTESIAN_POINT ( 'NONE',  ( 3.400026199384122538, 1.967065180803424740, -0.6696926287964158897 ) ) ;
#7153 = AXIS2_PLACEMENT_3D ( 'NONE', #12198, #542, #14417 ) ;
#7154 = LINE ( 'NONE', #150, #12270 ) ;
#7155 = DIRECTION ( 'NONE',  ( -1.000000000000000000, -0.000000000000000000, -0.000000000000000000 ) ) ;
#7156 = VERTEX_POINT ( 'NONE', #1002 ) ;
#7157 = DIRECTION ( 'NONE',  ( 0.000000000000000000, 0.000000000000000000, -1.000000000000000000 ) ) ;
#7158 = ORIENTED_EDGE ( 'NONE', *, *, #14769, .F. ) ;
#7159 = DIRECTION ( 'NONE',  ( 0.000000000000000000, 0.000000000000000000, -1.000000000000000000 ) ) ;
#7160 = ORIENTED_EDGE ( 'NONE', *, *, #696, .F. ) ;
#7161 = DIRECTION ( 'NONE',  ( 0.000000000000000000, 0.000000000000000000, -1.000000000000000000 ) ) ;
#7162 = LINE ( 'NONE', #3553, #3677 ) ;
#7163 = CARTESIAN_POINT ( 'NONE',  ( 0.007908111413600220699, -0.2214999999999999469, -0.5598942880828962076 ) ) ;
#7164 = DIRECTION ( 'NONE',  ( 0.000000000000000000, 0.000000000000000000, -1.000000000000000000 ) ) ;
#7165 = AXIS2_PLACEMENT_3D ( 'NONE', #1381, #5848, #13928 ) ;
#7166 = FILL_AREA_STYLE ('',( #10818 ) ) ;
#7167 = EDGE_LOOP ( 'NONE', ( #10918, #9091, #8946, #12726 ) ) ;
#7168 = EDGE_LOOP ( 'NONE', ( #9172, #2037, #13298, #2755 ) ) ;
#7169 = ORIENTED_EDGE ( 'NONE', *, *, #8594, .T. ) ;
#7170 = CARTESIAN_POINT ( 'NONE',  ( 3.426491571325181340, 2.005438169188070052, 0.6189082257615707849 ) ) ;
#7171 = LINE ( 'NONE', #8090, #2628 ) ;
#7172 = CARTESIAN_POINT ( 'NONE',  ( -0.4124999999999999223, 0.000000000000000000, 0.4124999999999999778 ) ) ;
#7173 = LINE ( 'NONE', #1329, #1408 ) ;
#7174 = VERTEX_POINT ( 'NONE', #5538 ) ;
#7175 = DIRECTION ( 'NONE',  ( 0.000000000000000000, 0.000000000000000000, 1.000000000000000000 ) ) ;
#7176 = EDGE_CURVE ( 'NONE', #12880, #8959, #3394, .T. ) ;
#7177 = COLOUR_RGB ( '',0.7921568627450980005, 0.8196078431372548767, 0.9333333333333333481 ) ;
#7178 = LINE ( 'NONE', #8398, #13395 ) ;
#7179 = CARTESIAN_POINT ( 'NONE',  ( 0.09500000000000431710, -1.679378605318047946, -2.054378605318054163 ) ) ;
#7180 = CARTESIAN_POINT ( 'NONE',  ( 3.874999999999999556, 3.170500000000001428, -1.509999999999999787 ) ) ;
#7181 = AXIS2_PLACEMENT_3D ( 'NONE', #2505, #5725, #9324 ) ;
#7182 = VERTEX_POINT ( 'NONE', #6849 ) ;
#7184 = ORIENTED_EDGE ( 'NONE', *, *, #7956, .T. ) ;
#7183 = FACE_OUTER_BOUND ( 'NONE', #10837, .T. ) ;
#7185 = ORIENTED_EDGE ( 'NONE', *, *, #4221, .F. ) ;
#7186 = CARTESIAN_POINT ( 'NONE',  ( -5.764454660286586870E-18, 0.06000000000000001166, 0.000000000000000000 ) ) ;
#7187 = ORIENTED_EDGE ( 'NONE', *, *, #12485, .F. ) ;
#7188 = FACE_OUTER_BOUND ( 'NONE', #7421, .T. ) ;
#7189 =( NAMED_UNIT ( * ) SI_UNIT ( $, .STERADIAN. ) SOLID_ANGLE_UNIT ( ) );
#7190 = FACE_BOUND ( 'NONE', #8626, .T. ) ;
#7191 = EDGE_LOOP ( 'NONE', ( #13644, #9560 ) ) ;
#7192 = CIRCLE ( 'NONE', #6212, 0.2944999999999979301 ) ;
#7193 = CARTESIAN_POINT ( 'NONE',  ( -0.09035531712817639061, 1.629999999999999893, 0.1565000000000000280 ) ) ;
#7194 = FACE_OUTER_BOUND ( 'NONE', #8607, .T. ) ;
#7195 = EDGE_CURVE ( 'NONE', #5706, #14916, #4541, .T. ) ;
#7196 = AXIS2_PLACEMENT_3D ( 'NONE', #5451, #7741, #4226 ) ;
#7197 = DIRECTION ( 'NONE',  ( 0.000000000000000000, 0.000000000000000000, -1.000000000000000000 ) ) ;
#7198 = EDGE_CURVE ( 'NONE', #6823, #9279, #12478, .T. ) ;
#7199 = CARTESIAN_POINT ( 'NONE',  ( 8.517841687953398022, 0.8704007761502550178, 0.3197150928555234639 ) ) ;
#7200 = DIRECTION ( 'NONE',  ( 0.000000000000000000, 0.000000000000000000, 1.000000000000000000 ) ) ;
#7201 = ADVANCED_FACE ( 'NONE', ( #13932 ), #2013, .F. ) ;
#7202 = CIRCLE ( 'NONE', #9873, 0.03999999999999998002 ) ;
#7203 = CARTESIAN_POINT ( 'NONE',  ( 0.000000000000000000, 0.000000000000000000, 0.5000000000000000000 ) ) ;
#7204 = CARTESIAN_POINT ( 'NONE',  ( 4.500347009044375568, 1.711009772181913968, 0.5018703121815807355 ) ) ;
#7205 = EDGE_CURVE ( 'NONE', #1593, #788, #10108, .T. ) ;
#7206 =( GEOMETRIC_REPRESENTATION_CONTEXT ( 3 ) GLOBAL_UNCERTAINTY_ASSIGNED_CONTEXT ( ( #8328 ) ) GLOBAL_UNIT_ASSIGNED_CONTEXT ( ( #14300, #285, #10866 ) ) REPRESENTATION_CONTEXT ( 'NONE', 'WORKASPACE' ) );
#7207 = EDGE_LOOP ( 'NONE', ( #10144, #12079, #14972, #2015 ) ) ;
#7208 = DIRECTION ( 'NONE',  ( -0.000000000000000000, -9.182682331643740718E-16, 1.000000000000000000 ) ) ;
#7210 = ORIENTED_EDGE ( 'NONE', *, *, #5456, .T. ) ;
#7209 = DIRECTION ( 'NONE',  ( 0.3420201433256627732, 0.000000000000000000, 0.9396926207859105373 ) ) ;
#7211 = ORIENTED_EDGE ( 'NONE', *, *, #15069, .F. ) ;
#7212 = CARTESIAN_POINT ( 'NONE',  ( 3.875000000000000000, 0.7099999999999984102, 0.4849999999999995981 ) ) ;
#7213 = CARTESIAN_POINT ( 'NONE',  ( 3.045371920833451096, 0.6267721954701777065, 0.3972696057388188096 ) ) ;
#7214 = ORIENTED_EDGE ( 'NONE', *, *, #11480, .F. ) ;
#7215 = CARTESIAN_POINT ( 'NONE',  ( 1.000000000000000222, -0.4429999999999998939, 0.4258697216429003785 ) ) ;
#7216 = CIRCLE ( 'NONE', #13531, 0.9999999999999996669 ) ;
#7217 = CARTESIAN_POINT ( 'NONE',  ( 3.426491571325181340, -2.359999999999984333, 1.575000000000016387 ) ) ;
#7218 = DIRECTION ( 'NONE',  ( 0.000000000000000000, -1.000000000000000000, -0.000000000000000000 ) ) ;
#7219 = EDGE_CURVE ( 'NONE', #14571, #7869, #11814, .T. ) ;
#7220 = ORIENTED_EDGE ( 'NONE', *, *, #6240, .T. ) ;
#7221 = CARTESIAN_POINT ( 'NONE',  ( 0.6566433263007029897, -0.4313127572425527467, 0.4973513887421178725 ) ) ;
#7222 = DIRECTION ( 'NONE',  ( -0.9999002670844989726, 2.602203049398214110E-17, 0.01412288512831212997 ) ) ;
#7223 = CARTESIAN_POINT ( 'NONE',  ( 0.09500000000000431710, 1.679378605318035733, -1.679378605318065487 ) ) ;
#7224 = ADVANCED_FACE ( 'NONE', ( #923 ), #8933, .F. ) ;
#7225 = ORIENTED_EDGE ( 'NONE', *, *, #2104, .T. ) ;
#7226 = FACE_OUTER_BOUND ( 'NONE', #14700, .T. ) ;
#7227 = VERTEX_POINT ( 'NONE', #13773 ) ;
#7228 = AXIS2_PLACEMENT_3D ( 'NONE', #6681, #5387, #5619 ) ;
#7229 = VECTOR ( 'NONE', #13079, 39.37007874015748143 ) ;
#7230 = EDGE_CURVE ( 'NONE', #5886, #193, #1995, .T. ) ;
#7231 = CARTESIAN_POINT ( 'NONE',  ( -0.2099999999999948852, 1.559103846021543616, 0.3809527529760087239 ) ) ;
#7232 = ORIENTED_EDGE ( 'NONE', *, *, #5218, .T. ) ;
#7233 = DIRECTION ( 'NONE',  ( -0.7071067811865455743, 0.000000000000000000, 0.7071067811865493491 ) ) ;
#7234 = FACE_OUTER_BOUND ( 'NONE', #7499, .T. ) ;
#7235 = AXIS2_PLACEMENT_3D ( 'NONE', #10204, #3469, #8072 ) ;
#7236 = CARTESIAN_POINT ( 'NONE',  ( 2.414213562373087374, 0.1427864376268978830, 0.4064941968476759038 ) ) ;
#7237 = VECTOR ( 'NONE', #8079, 39.37007874015748143 ) ;
#7238 = CIRCLE ( 'NONE', #9182, 0.2432499999999999385 ) ;
#7239 = CARTESIAN_POINT ( 'NONE',  ( 2.774999999999999911, -1.679378605318041950, 1.416878605318058870 ) ) ;
#7240 = ORIENTED_EDGE ( 'NONE', *, *, #7055, .T. ) ;
#7241 = ORIENTED_EDGE ( 'NONE', *, *, #11203, .F. ) ;
#7242 = ORIENTED_EDGE ( 'NONE', *, *, #6414, .F. ) ;
#7243 = ADVANCED_FACE ( 'NONE', ( #3316 ), #3564, .F. ) ;
#7244 = VECTOR ( 'NONE', #5521, 39.37007874015748143 ) ;
#7245 = FACE_OUTER_BOUND ( 'NONE', #4184, .T. ) ;
#7246 = DIRECTION ( 'NONE',  ( 0.000000000000000000, -1.000000000000000000, -4.591341165822158293E-16 ) ) ;
#7247 = AXIS2_PLACEMENT_3D ( 'NONE', #3786, #6930, #11586 ) ;
#7248 = CIRCLE ( 'NONE', #2086, 0.4070000000000046914 ) ;
#7249 = CARTESIAN_POINT ( 'NONE',  ( 1.000847373107698779, -0.3829999999999998961, 0.4858637376679703634 ) ) ;
#7250 = CARTESIAN_POINT ( 'NONE',  ( 2.774999999999999911, 0.9800000000000039790, 2.359999999999999876 ) ) ;
#7251 = EDGE_LOOP ( 'NONE', ( #10335, #752 ) ) ;
#7252 = DIRECTION ( 'NONE',  ( -0.7071067811865350272, -0.7071067811865600072, 0.000000000000000000 ) ) ;
#7253 = CARTESIAN_POINT ( 'NONE',  ( 1.612492615670230611, 0.05745813234176449374, 0.4169456318805255801 ) ) ;
#7254 = PLANE ( 'NONE',  #9799 ) ;
#7255 = AXIS2_PLACEMENT_3D ( 'NONE', #2116, #6801, #3048 ) ;
#7256 = CARTESIAN_POINT ( 'NONE',  ( 4.310174322509690015, 1.779561302064900596, -0.6129903542706727215 ) ) ;
#7257 = ORIENTED_EDGE ( 'NONE', *, *, #1393, .T. ) ;
#7259 = ORIENTED_EDGE ( 'NONE', *, *, #3844, .T. ) ;
#7258 = DIRECTION ( 'NONE',  ( -1.000000000000000000, -0.000000000000000000, -0.000000000000000000 ) ) ;
#7260 = VERTEX_POINT ( 'NONE', #12715 ) ;
#7261 = CARTESIAN_POINT ( 'NONE',  ( 0.3724999999999999423, 0.2159999999999999420, 0.3724999999999999423 ) ) ;
#7262 = ORIENTED_EDGE ( 'NONE', *, *, #11669, .F. ) ;
#7263 = ADVANCED_FACE ( 'NONE', ( #1077 ), #9059, .F. ) ;
#7264 = CIRCLE ( 'NONE', #1611, 0.2812500000000000555 ) ;
#7265 =( NAMED_UNIT ( * ) PLANE_ANGLE_UNIT ( ) SI_UNIT ( $, .RADIAN. ) );
#7266 = CARTESIAN_POINT ( 'NONE',  ( 0.8999999999999998002, 0.1749999999999999889, -0.3799999999999999489 ) ) ;
#7267 = VERTEX_POINT ( 'NONE', #2157 ) ;
#7268 = LINE ( 'NONE', #6039, #12629 ) ;
#7269 = FACE_OUTER_BOUND ( 'NONE', #2364, .T. ) ;
#7270 = CYLINDRICAL_SURFACE ( 'NONE', #1215, 0.1249999999999999861 ) ;
#7271 = AXIS2_PLACEMENT_3D ( 'NONE', #1790, #14730, #11363 ) ;
#7272 = PRODUCT_DEFINITION_SHAPE ( 'NONE', 'NONE',  #1525 ) ;
#7273 = CARTESIAN_POINT ( 'NONE',  ( 8.573547510565930452, 0.9318103594813683666, 0.3691840008912894988 ) ) ;
#7274 = VECTOR ( 'NONE', #6556, 39.37007874015748143 ) ;
#7275 =( BOUNDED_SURFACE ( )  B_SPLINE_SURFACE ( 3, 2, ( 
 ( #14193, #7110, #4722 ),
 ( #2429, #1411, #3576 ),
 ( #5027, #2575, #181 ),
 ( #11757, #13114, #8337 ),
 ( #14340, #319, #7253 ),
 ( #14116, #4800, #2651 ),
 ( #9472, #6106, #2498 ),
 ( #12891, #3876, #12969 ),
 ( #12049, #9549, #3655 ),
 ( #7397, #13187, #1333 ) ),
 .UNSPECIFIED., .F., .F., .F. ) 
 B_SPLINE_SURFACE_WITH_KNOTS ( ( 4, 2, 2, 2, 4 ),
 ( 3, 3 ),
 ( 4.712388980384689674, 4.908738521234051966, 5.105088062083414258, 5.301437602932777438, 5.497787143782139729 ),
 ( 0.000000000000000000, 1.000000000000000000 ),
 .UNSPECIFIED. ) 
 GEOMETRIC_REPRESENTATION_ITEM ( )  RATIONAL_B_SPLINE_SURFACE ( (
 ( 1.000000000000000000, 0.7071067811865475727, 1.000000000000000000),
 ( 1.000000000000000000, 0.7067799747774232699, 1.000000000000000000),
 ( 1.000000000000000000, 0.7064529522741163081, 1.000000000000000000),
 ( 1.000000000000000000, 0.7058110186552004617, 1.000000000000000000),
 ( 1.000000000000000000, 0.7054961263470524990, 1.000000000000000000),
 ( 1.000000000000000000, 0.7048906332647922879, 1.000000000000000000),
 ( 1.000000000000000000, 0.7046000480551916079, 1.000000000000000000),
 ( 1.000000000000000000, 0.7040544485608896119, 1.000000000000000000),
 ( 1.000000000000000000, 0.7037994241814393703, 1.000000000000000000),
 ( 1.000000000000000000, 0.7035672008258526677, 1.000000000000000000) ) ) 
 REPRESENTATION_ITEM ( '' )  SURFACE ( )  );
#7276 = CARTESIAN_POINT ( 'NONE',  ( 3.574207760192867678, 1.912292896761111471, 0.6869911351339433869 ) ) ;
#7277 = EDGE_CURVE ( 'NONE', #11902, #8264, #121, .T. ) ;
#7278 = CARTESIAN_POINT ( 'NONE',  ( 0.000000000000000000, 1.559103846021539619, 0.000000000000000000 ) ) ;
#7279 = ADVANCED_FACE ( 'NONE', ( #9211 ), #5462, .T. ) ;
#7280 = ORIENTED_EDGE ( 'NONE', *, *, #6418, .F. ) ;
#7281 = EDGE_CURVE ( 'NONE', #5452, #2763, #5765, .T. ) ;
#7282 = LINE ( 'NONE', #10935, #14305 ) ;
#7284 = ORIENTED_EDGE ( 'NONE', *, *, #4947, .F. ) ;
#7283 = CARTESIAN_POINT ( 'NONE',  ( 0.000000000000000000, 0.000000000000000000, 0.000000000000000000 ) ) ;
#7285 = VERTEX_POINT ( 'NONE', #10429 ) ;
#7286 = VECTOR ( 'NONE', #6339, 39.37007874015748143 ) ;
#7287 = DIRECTION ( 'NONE',  ( -0.7070715176384863021, -0.7070715176384774203, 0.009986885842351498482 ) ) ;
#7288 = CARTESIAN_POINT ( 'NONE',  ( 2.124999999999999556, 0.9799999999999436939, -3.360000000000016751 ) ) ;
#7289 = CARTESIAN_POINT ( 'NONE',  ( 2.633946444925666430, 0.3625193201794738584, 0.4033906250602100618 ) ) ;
#7290 = EDGE_LOOP ( 'NONE', ( #12519, #1911, #7574, #2620 ) ) ;
#7291 = LINE ( 'NONE', #141, #4118 ) ;
#7292 = ADVANCED_FACE ( 'NONE', ( #15091 ), #12583, .T. ) ;
#7293 = AXIS2_PLACEMENT_3D ( 'NONE', #1543, #7594, #9971 ) ;
#7294 = FACE_OUTER_BOUND ( 'NONE', #6610, .T. ) ;
#7295 = DIRECTION ( 'NONE',  ( 0.000000000000000000, 0.000000000000000000, -1.000000000000000000 ) ) ;
#7296 = AXIS2_PLACEMENT_3D ( 'NONE', #13895, #12520, #9174 ) ;
#7297 = VERTEX_POINT ( 'NONE', #3704 ) ;
#7298 = DIRECTION ( 'NONE',  ( -0.7071067811865459074, 0.000000000000000000, 0.7071067811865490160 ) ) ;
#7299 = CARTESIAN_POINT ( 'NONE',  ( 3.426491571325181340, 1.679378605318059048, 1.973878605318039492 ) ) ;
#7300 = LINE ( 'NONE', #227, #11709 ) ;
#7301 = VERTEX_POINT ( 'NONE', #5852 ) ;
#7302 = CIRCLE ( 'NONE', #8021, 0.06000000000000001166 ) ;
#7303 = CARTESIAN_POINT ( 'NONE',  ( 3.875000000000000000, 3.137999999999999901, 0.000000000000000000 ) ) ;
#7304 = VERTEX_POINT ( 'NONE', #1466 ) ;
#7305 = VECTOR ( 'NONE', #1371, 39.37007874015748143 ) ;
#7306 = CARTESIAN_POINT ( 'NONE',  ( -0.3117353328467220019, 1.602948811930424267, 0.2219640709470993845 ) ) ;
#7307 = ORIENTED_EDGE ( 'NONE', *, *, #1582, .T. ) ;
#7308 = AXIS2_PLACEMENT_3D ( 'NONE', #10344, #996, #1149 ) ;
#7309 = AXIS2_PLACEMENT_3D ( 'NONE', #1698, #1395, #5085 ) ;
#7310 = EDGE_CURVE ( 'NONE', #1160, #8873, #14008, .T. ) ;
#7311 = DIRECTION ( 'NONE',  ( 0.000000000000000000, 0.000000000000000000, -1.000000000000000000 ) ) ;
#7312 = CIRCLE ( 'NONE', #4135, 0.03999999999999998002 ) ;
#7313 = CARTESIAN_POINT ( 'NONE',  ( 3.426491571325181340, -0.9799999999999989830, -2.359999999999999876 ) ) ;
#7314 = AXIS2_PLACEMENT_3D ( 'NONE', #14498, #7624, #10080 ) ;
#7315 = EDGE_CURVE ( 'NONE', #6090, #6255, #14793, .T. ) ;
#7316 = DIRECTION ( 'NONE',  ( 1.000000000000000000, 0.000000000000000000, 0.000000000000000000 ) ) ;
#7317 = CIRCLE ( 'NONE', #14626, 0.1249999999999999029 ) ;
#7318 = ORIENTED_EDGE ( 'NONE', *, *, #8982, .F. ) ;
#7319 = ORIENTED_EDGE ( 'NONE', *, *, #8373, .F. ) ;
#7320 = VECTOR ( 'NONE', #3603, 39.37007874015748143 ) ;
#7321 = EDGE_LOOP ( 'NONE', ( #9428, #4293, #3803, #9936 ) ) ;
#7322 = CARTESIAN_POINT ( 'NONE',  ( -0.4124999999999999223, 0.1749999999999999889, 0.4124999999999999778 ) ) ;
#7323 = CARTESIAN_POINT ( 'NONE',  ( 3.426491571325181340, 0.9799999999999436939, -3.360000000000016751 ) ) ;
#7324 = DIRECTION ( 'NONE',  ( -0.000000000000000000, -1.000000000000000000, -0.000000000000000000 ) ) ;
#7325 = DIRECTION ( 'NONE',  ( -1.000000000000000000, -0.000000000000000000, -0.000000000000000000 ) ) ;
#7326 = VECTOR ( 'NONE', #13857, 39.37007874015748143 ) ;
#7327 = CARTESIAN_POINT ( 'NONE',  ( 3.863498198434387909, 1.886760551146561271, -0.5000000000000004441 ) ) ;
#7328 = LINE ( 'NONE', #30, #3653 ) ;
#7329 = FILL_AREA_STYLE ('',( #6107 ) ) ;
#7330 = EDGE_CURVE ( 'NONE', #7375, #392, #12947, .T. ) ;
#7331 = ADVANCED_FACE ( 'NONE', ( #10742 ), #2477, .F. ) ;
#7332 = AXIS2_PLACEMENT_3D ( 'NONE', #13996, #2385, #9356 ) ;
#7333 = ORIENTED_EDGE ( 'NONE', *, *, #3102, .T. ) ;
#7335 = ORIENTED_EDGE ( 'NONE', *, *, #10637, .F. ) ;
#7334 = LINE ( 'NONE', #8405, #2765 ) ;
#7336 = ORIENTED_EDGE ( 'NONE', *, *, #2611, .T. ) ;
#7337 = DIRECTION ( 'NONE',  ( -1.000000000000000000, -1.365923996832131609E-16, 0.000000000000000000 ) ) ;
#7338 = DIRECTION ( 'NONE',  ( 1.365923996832131609E-16, -1.000000000000000000, -0.000000000000000000 ) ) ;
#7339 = DIRECTION ( 'NONE',  ( -0.9994005049267692398, -2.319470939493371467E-15, -0.03462124711964004870 ) ) ;
#7340 = CARTESIAN_POINT ( 'NONE',  ( 2.381934877626968206, 0.6476033094210934538, 0.4663568520109472870 ) ) ;
#7341 = EDGE_LOOP ( 'NONE', ( #7388, #58, #11635, #14345 ) ) ;
#7342 = CARTESIAN_POINT ( 'NONE',  ( -0.2028461515626820144, 1.564725569476186573, -0.3809527529760086684 ) ) ;
#7343 = CARTESIAN_POINT ( 'NONE',  ( 0.000000000000000000, 1.591999999999999638, 0.000000000000000000 ) ) ;
#7344 = VECTOR ( 'NONE', #7839, 39.37007874015748854 ) ;
#7345 = DIRECTION ( 'NONE',  ( -1.000000000000000000, -0.000000000000000000, -0.000000000000000000 ) ) ;
#7346 = CARTESIAN_POINT ( 'NONE',  ( 3.426491571325181340, -2.399999999999999911, 0.7000000000000007327 ) ) ;
#7347 = FACE_BOUND ( 'NONE', #13995, .T. ) ;
#7348 = CARTESIAN_POINT ( 'NONE',  ( 0.8352936206970669186, -0.4446654365634041262, -0.4130780710220839369 ) ) ;
#7349 =( REPRESENTATION_RELATIONSHIP ('NONE','NONE', #3591, #1600 ) REPRESENTATION_RELATIONSHIP_WITH_TRANSFORMATION ( #7699 )SHAPE_REPRESENTATION_RELATIONSHIP( ) );
#7350 = CARTESIAN_POINT ( 'NONE',  ( 3.596711980515629570, 1.970780182464999530, 0.6960332242240829803 ) ) ;
#7351 = DIRECTION ( 'NONE',  ( 0.000000000000000000, 0.000000000000000000, -1.000000000000000000 ) ) ;
#7352 = ORIENTED_EDGE ( 'NONE', *, *, #1667, .T. ) ;
#7353 = CARTESIAN_POINT ( 'NONE',  ( 0.4424999999999979505, -0.6589999999999996971, -0.8500000000000000888 ) ) ;
#7355 = VERTEX_POINT ( 'NONE', #5004 ) ;
#7354 = CARTESIAN_POINT ( 'NONE',  ( 6.826491571325181695, 1.679378605318035733, -1.679378605318065487 ) ) ;
#7356 = VERTEX_POINT ( 'NONE', #5997 ) ;
#7357 = DIRECTION ( 'NONE',  ( -0.000000000000000000, -1.000000000000000000, -0.000000000000000000 ) ) ;
#7358 = DIRECTION ( 'NONE',  ( 0.000000000000000000, 0.000000000000000000, 1.000000000000000000 ) ) ;
#7359 = CARTESIAN_POINT ( 'NONE',  ( 2.738674485064839459, 0.4577639129046877642, 0.4613181569904871160 ) ) ;
#7360 = ORIENTED_EDGE ( 'NONE', *, *, #12956, .T. ) ;
#7361 = FACE_OUTER_BOUND ( 'NONE', #10495, .T. ) ;
#7362 = AXIS2_PLACEMENT_3D ( 'NONE', #5418, #10082, #13578 ) ;
#7363 = EDGE_CURVE ( 'NONE', #3991, #14644, #592, .T. ) ;
#7364 = CARTESIAN_POINT ( 'NONE',  ( 0.7040121242107247879, -0.05591482235280140212, 0.4900563259292270990 ) ) ;
#7365 = EDGE_CURVE ( 'NONE', #331, #159, #5519, .T. ) ;
#7366 =( BOUNDED_CURVE ( )  B_SPLINE_CURVE ( 3, ( #10920, #14277, #483, #9921 ),
 .UNSPECIFIED., .F., .F. ) 
 B_SPLINE_CURVE_WITH_KNOTS ( ( 4, 4 ),
 ( 1.570796326794896780, 2.356194490192346613 ),
 .UNSPECIFIED. ) 
 CURVE ( )  GEOMETRIC_REPRESENTATION_ITEM ( )  RATIONAL_B_SPLINE_CURVE ( ( 1.000000000000000000, 0.9492530216741910110, 0.9492530216741910110, 1.000000000000000000 ) ) 
 REPRESENTATION_ITEM ( '' )  );
#7367 = DIRECTION ( 'NONE',  ( -0.9999002670844990837, 0.000000000000000000, 0.01412288512831215426 ) ) ;
#7368 = VERTEX_POINT ( 'NONE', #6074 ) ;
#7369 = DIRECTION ( 'NONE',  ( -0.000000000000000000, -1.000000000000000000, -0.000000000000000000 ) ) ;
#7370 = CYLINDRICAL_SURFACE ( 'NONE', #13482, 0.08500000000000004774 ) ;
#7371 = CARTESIAN_POINT ( 'NONE',  ( 0.7243146799153700188, -0.2214999999999999469, 0.4897695666678619220 ) ) ;
#7372 = ADVANCED_FACE ( 'NONE', ( #7226 ), #7, .T. ) ;
#7373=STYLED_ITEM('',(#15199),#5616);
#7374 = CARTESIAN_POINT ( 'NONE',  ( 2.774999999999999911, -0.9799999999999436939, 3.360000000000016751 ) ) ;
#7375 = VERTEX_POINT ( 'NONE', #10662 ) ;
#7376 = CARTESIAN_POINT ( 'NONE',  ( 0.7020310496751535068, -0.02903435051206633769, 0.4816878228448820409 ) ) ;
#7377 = EDGE_LOOP ( 'NONE', ( #4847, #10943, #1774, #14240 ) ) ;
#7378 = DIRECTION ( 'NONE',  ( -0.000000000000000000, 0.000000000000000000, 1.000000000000000000 ) ) ;
#7379 = FACE_OUTER_BOUND ( 'NONE', #13045, .T. ) ;
#7380 = EDGE_CURVE ( 'NONE', #7890, #2690, #4535, .T. ) ;
#7381 = CARTESIAN_POINT ( 'NONE',  ( 0.7856509485162607165, -0.4429999999999998939, -0.3627813902276395552 ) ) ;
#7382 = EDGE_CURVE ( 'NONE', #1793, #13688, #9523, .T. ) ;
#7383 = VECTOR ( 'NONE', #3322, 39.37007874015748143 ) ;
#7384 = CYLINDRICAL_SURFACE ( 'NONE', #1415, 0.4849999999999995981 ) ;
#7385 = FACE_OUTER_BOUND ( 'NONE', #6518, .T. ) ;
#7386 = EDGE_LOOP ( 'NONE', ( #11174, #9446, #7529, #13104 ) ) ;
#7387 = VERTEX_POINT ( 'NONE', #14170 ) ;
#7388 = ORIENTED_EDGE ( 'NONE', *, *, #7727, .T. ) ;
#7389 = EDGE_CURVE ( 'NONE', #13163, #12635, #11121, .T. ) ;
#7390 = CARTESIAN_POINT ( 'NONE',  ( 8.705855184453682227, 0.9357017671274362458, -0.3021636316005746892 ) ) ;
#7391 = CIRCLE ( 'NONE', #757, 0.4349999999999999423 ) ;
#7392 = CARTESIAN_POINT ( 'NONE',  ( 0.8999999999999998002, 0.000000000000000000, -0.4850000000000000977 ) ) ;
#7393 = CARTESIAN_POINT ( 'NONE',  ( 0.06299999999999994493, -1.679378605318047946, -1.272378605318047917 ) ) ;
#7394 = EDGE_CURVE ( 'NONE', #11919, #11196, #11884, .T. ) ;
#7395 = DIRECTION ( 'NONE',  ( -0.000000000000000000, -0.000000000000000000, 1.000000000000000000 ) ) ;
#7396 = CARTESIAN_POINT ( 'NONE',  ( 3.426491571325181784, 1.978195973981552003, -0.6427388825267555950 ) ) ;
#7397 = CARTESIAN_POINT ( 'NONE',  ( 2.088768908813761094, 0.2870784642939447906, 0.4704976142822914764 ) ) ;
#7398 = AXIS2_PLACEMENT_3D ( 'NONE', #3539, #4767, #5920 ) ;
#7399 = EDGE_CURVE ( 'NONE', #9046, #7832, #2578, .T. ) ;
#7400 = VECTOR ( 'NONE', #7935, 39.37007874015748143 ) ;
#7401 = VERTEX_POINT ( 'NONE', #9369 ) ;
#7402 = ORIENTED_EDGE ( 'NONE', *, *, #5942, .F. ) ;
#7403 = ORIENTED_EDGE ( 'NONE', *, *, #8358, .F. ) ;
#7404 = CARTESIAN_POINT ( 'NONE',  ( 0.009170202274340883905, 1.603403463250997918, 0.3809527529760087239 ) ) ;
#7405 = PLANE ( 'NONE',  #4823 ) ;
#7406 = CARTESIAN_POINT ( 'NONE',  ( 4.322740670651102235, 0.9748968923800885866, -0.2231469905907089712 ) ) ;
#7407 = EDGE_CURVE ( 'NONE', #3954, #11196, #9906, .T. ) ;
#7408 = VERTEX_POINT ( 'NONE', #1235 ) ;
#7409 = CARTESIAN_POINT ( 'NONE',  ( 0.000000000000000000, 0.000000000000000000, 0.000000000000000000 ) ) ;
#7410 = CARTESIAN_POINT ( 'NONE',  ( 6.794491571325179891, -1.679378605318048390, 2.054378605318054607 ) ) ;
#7411 = DIRECTION ( 'NONE',  ( 0.000000000000000000, 0.000000000000000000, 1.000000000000000000 ) ) ;
#7412 = AXIS2_PLACEMENT_3D ( 'NONE', #11534, #11767, #1035 ) ;
#7413 = DIRECTION ( 'NONE',  ( 0.000000000000000000, 1.000000000000000000, 0.000000000000000000 ) ) ;
#7414 = DIRECTION ( 'NONE',  ( 0.000000000000000000, -1.000000000000000000, 0.000000000000000000 ) ) ;
#7415 = DIRECTION ( 'NONE',  ( 0.000000000000000000, 1.000000000000000000, -0.000000000000000000 ) ) ;
#7416 = DIRECTION ( 'NONE',  ( -1.000000000000000000, -0.000000000000000000, -0.000000000000000000 ) ) ;
#7417 = VERTEX_POINT ( 'NONE', #1309 ) ;
#7418 = AXIS2_PLACEMENT_3D ( 'NONE', #7598, #258, #9897 ) ;
#7419 = PLANE ( 'NONE',  #7969 ) ;
#7421 = EDGE_LOOP ( 'NONE', ( #9738, #591, #516, #8698, #12661, #1956 ) ) ;
#7420 = DIRECTION ( 'NONE',  ( 0.7071067811865354713, -0.7071067811865595631, 0.000000000000000000 ) ) ;
#7422 = ORIENTED_EDGE ( 'NONE', *, *, #9756, .T. ) ;
#7423 = AXIS2_PLACEMENT_3D ( 'NONE', #9670, #299, #13306 ) ;
#7424 = CARTESIAN_POINT ( 'NONE',  ( 0.000000000000000000, 0.000000000000000000, 0.000000000000000000 ) ) ;
#7425 = EDGE_CURVE ( 'NONE', #4452, #5805, #8524, .T. ) ;
#7426 = PLANE ( 'NONE',  #4524 ) ;
#7427 = ORIENTED_EDGE ( 'NONE', *, *, #10554, .F. ) ;
#7428 = CARTESIAN_POINT ( 'NONE',  ( 3.426491571325181340, 0.000000000000000000, 0.000000000000000000 ) ) ;
#7429 = CARTESIAN_POINT ( 'NONE',  ( 0.6555286510801312527, -0.04031751147701368582, 0.5099168278768518858 ) ) ;
#7430 = CONICAL_SURFACE ( 'NONE', #83, 0.2219999999999999751, 0.7853981633974349563 ) ;
#7431 = DIRECTION ( 'NONE',  ( -1.000000000000000000, -0.000000000000000000, -0.000000000000000000 ) ) ;
#7432 = CIRCLE ( 'NONE', #6949, 0.06000000000000001860 ) ;
#7433 = ORIENTED_EDGE ( 'NONE', *, *, #13123, .T. ) ;
#7434 = CARTESIAN_POINT ( 'NONE',  ( 2.774999999999999911, 1.679378605318042395, -1.384878605318057732 ) ) ;
#7435 = LINE ( 'NONE', #12092, #1998 ) ;
#7436 = LENGTH_MEASURE_WITH_UNIT ( LENGTH_MEASURE( 0.02539999999999999897 ), #4064 );
#7437 = DIRECTION ( 'NONE',  ( -0.000000000000000000, -1.000000000000000000, -0.000000000000000000 ) ) ;
#7438 = ORIENTED_EDGE ( 'NONE', *, *, #13062, .F. ) ;
#7439 = CARTESIAN_POINT ( 'NONE',  ( -0.2448097035963034407, 1.581125151349165314, 0.3378826611373411115 ) ) ;
#7440 = ORIENTED_EDGE ( 'NONE', *, *, #3326, .F. ) ;
#7441 = VECTOR ( 'NONE', #11421, 39.37007874015748143 ) ;
#7442 = FACE_OUTER_BOUND ( 'NONE', #9072, .T. ) ;
#7443 = PRODUCT_DEFINITION_FORMATION_WITH_SPECIFIED_SOURCE ( 'ANY', '', #1752, .NOT_KNOWN. ) ;
#7444 = CARTESIAN_POINT ( 'NONE',  ( 2.633946444925666874, 0.3625193201794746356, 0.5000000000000000000 ) ) ;
#7445 = CARTESIAN_POINT ( 'NONE',  ( 0.8293604527229431200, -0.4837317850455687962, -0.3495425184068792768 ) ) ;
#7446 = DIRECTION ( 'NONE',  ( -1.000000000000000000, -0.000000000000000000, -0.000000000000000000 ) ) ;
#7447 = AXIS2_PLACEMENT_3D ( 'NONE', #1404, #2644, #394 ) ;
#7448 = CARTESIAN_POINT ( 'NONE',  ( 4.769999282678940657E-17, 1.610000000000000098, 0.3440000000000000280 ) ) ;
#7449 = DIRECTION ( 'NONE',  ( 0.000000000000000000, 0.000000000000000000, -1.000000000000000000 ) ) ;
#7450 = DIMENSIONAL_EXPONENTS ( 1.000000000000000000, 0.000000000000000000, 0.000000000000000000, 0.000000000000000000, 0.000000000000000000, 0.000000000000000000, 0.000000000000000000 ) ;
#7451 = CONICAL_SURFACE ( 'NONE', #11351, 0.4070000000000025264, 0.7853981633974557175 ) ;
#7452 = VECTOR ( 'NONE', #13844, 39.37007874015748854 ) ;
#7453 = ORIENTED_EDGE ( 'NONE', *, *, #11288, .T. ) ;
#7454 = ORIENTED_EDGE ( 'NONE', *, *, #13698, .F. ) ;
#7455 = EDGE_CURVE ( 'NONE', #15103, #4834, #6486, .T. ) ;
#7456 = ORIENTED_EDGE ( 'NONE', *, *, #10810, .T. ) ;
#7457 = ADVANCED_FACE ( 'NONE', ( #79 ), #14091, .F. ) ;
#7458 = FACE_OUTER_BOUND ( 'NONE', #5016, .T. ) ;
#7459 = ADVANCED_FACE ( 'NONE', ( #2769 ), #675, .T. ) ;
#7460 = CARTESIAN_POINT ( 'NONE',  ( -0.1807106342563527812, 1.629999999999999893, 3.262375646219079751E-17 ) ) ;
#7461 = VECTOR ( 'NONE', #968, 39.37007874015748143 ) ;
#7462 = DIRECTION ( 'NONE',  ( 0.000000000000000000, 0.000000000000000000, 1.000000000000000000 ) ) ;
#7463 = CARTESIAN_POINT ( 'NONE',  ( 3.426491571325181784, 2.032414231895940393, -0.6051366186278370751 ) ) ;
#7464 = VECTOR ( 'NONE', #11888, 39.37007874015748143 ) ;
#7465 = AXIS2_PLACEMENT_3D ( 'NONE', #3450, #13914, #12698 ) ;
#7466 = EDGE_CURVE ( 'NONE', #10168, #557, #7586, .T. ) ;
#7467 = CARTESIAN_POINT ( 'NONE',  ( 4.422240817987284522, 1.782290669966776209, -0.5151263722802654765 ) ) ;
#7468 = CARTESIAN_POINT ( 'NONE',  ( 2.372634528609593563, 0.1852128444980908617, 0.4664882128727458888 ) ) ;
#7469 = ORIENTED_EDGE ( 'NONE', *, *, #12294, .T. ) ;
#7470 = AXIS2_PLACEMENT_3D ( 'NONE', #7131, #9343, #15145 ) ;
#7471 = ORIENTED_EDGE ( 'NONE', *, *, #5411, .F. ) ;
#7472 = VECTOR ( 'NONE', #7921, 39.37007874015748143 ) ;
#7473 = ORIENTED_EDGE ( 'NONE', *, *, #7195, .T. ) ;
#7474 = CARTESIAN_POINT ( 'NONE',  ( 2.774999999999999911, -1.679378605318059048, -1.679378605318041950 ) ) ;
#7475 = CARTESIAN_POINT ( 'NONE',  ( 4.769268701363833074, 2.750000000000000000, 0.3249191361593796734 ) ) ;
#7476 = DIRECTION ( 'NONE',  ( -0.8660254037844388186, 0.000000000000000000, 0.4999999999999998335 ) ) ;
#7477 = DIRECTION ( 'NONE',  ( 0.000000000000000000, 0.000000000000000000, 1.000000000000000000 ) ) ;
#7478 = FACE_OUTER_BOUND ( 'NONE', #7341, .T. ) ;
#7479 = ORIENTED_EDGE ( 'NONE', *, *, #9134, .F. ) ;
#7480 = DIRECTION ( 'NONE',  ( -0.9999002670844991947, 0.000000000000000000, 0.01412288512831128343 ) ) ;
#7481 = DIRECTION ( 'NONE',  ( 0.000000000000000000, 1.000000000000000000, 0.000000000000000000 ) ) ;
#7482 = CIRCLE ( 'NONE', #1840, 0.1899999999999996136 ) ;
#7483 = DIRECTION ( 'NONE',  ( 0.000000000000000000, 0.000000000000000000, -1.000000000000000000 ) ) ;
#7484 = ADVANCED_FACE ( 'NONE', ( #5150 ), #2830, .F. ) ;
#7485 = CIRCLE ( 'NONE', #12849, 0.03999999999999998695 ) ;
#7486 = CARTESIAN_POINT ( 'NONE',  ( 0.09035531712817648775, 1.629999999999999893, -0.1564999999999998892 ) ) ;
#7487 = CARTESIAN_POINT ( 'NONE',  ( 3.875000000000000000, 3.137999999999999901, 0.5000000000000002220 ) ) ;
#7488 = EDGE_CURVE ( 'NONE', #10132, #1776, #1829, .T. ) ;
#7489 = CARTESIAN_POINT ( 'NONE',  ( -0.09035531712817639061, 1.379999999999999671, 0.1565000000000000280 ) ) ;
#7490 = CARTESIAN_POINT ( 'NONE',  ( 3.497790632039259329, 1.947309111526952963, 0.6487173296532952049 ) ) ;
#7491 = CARTESIAN_POINT ( 'NONE',  ( 0.000000000000000000, 0.000000000000000000, 0.000000000000000000 ) ) ;
#7492 = ORIENTED_EDGE ( 'NONE', *, *, #11283, .F. ) ;
#7493 = CARTESIAN_POINT ( 'NONE',  ( 0.6566521509169380710, -0.4313701889023026648, 0.4973154343666586485 ) ) ;
#7495 = ORIENTED_EDGE ( 'NONE', *, *, #4381, .F. ) ;
#7494 = CARTESIAN_POINT ( 'NONE',  ( 0.4124999999999997558, -0.6290000000000003366, -0.3725000000000000533 ) ) ;
#7496 = ORIENTED_EDGE ( 'NONE', *, *, #12925, .F. ) ;
#7497 = CARTESIAN_POINT ( 'NONE',  ( 0.000000000000000000, 1.109999999999999876, -0.2499999999999999167 ) ) ;
#7498 = CARTESIAN_POINT ( 'NONE',  ( 0.000000000000000000, 0.000000000000000000, 0.000000000000000000 ) ) ;
#7499 = EDGE_LOOP ( 'NONE', ( #11286, #2511, #6832, #5552, #12540, #6536, #6833, #2799, #12055, #4257 ) ) ;
#7500 = CARTESIAN_POINT ( 'NONE',  ( 0.4108223460329293864, 5.750000000000000000, 1.434378554753729569E-15 ) ) ;
#7501 = DIRECTION ( 'NONE',  ( -0.000000000000000000, -1.000000000000000000, -0.000000000000000000 ) ) ;
#7502 = CONICAL_SURFACE ( 'NONE', #879, 0.07000000000000047851, 0.7853981633974297383 ) ;
#7503 = CARTESIAN_POINT ( 'NONE',  ( 2.124999999999999556, 1.679378605318059048, 1.973878605318041268 ) ) ;
#7504 = DIRECTION ( 'NONE',  ( 0.000000000000000000, 0.000000000000000000, -1.000000000000000000 ) ) ;
#7505 = ORIENTED_EDGE ( 'NONE', *, *, #11281, .T. ) ;
#7506 = EDGE_CURVE ( 'NONE', #13657, #14149, #11098, .T. ) ;
#7507 = DIRECTION ( 'NONE',  ( 0.000000000000000000, 0.000000000000000000, -1.000000000000000000 ) ) ;
#7508 = FACE_OUTER_BOUND ( 'NONE', #12901, .T. ) ;
#7509 = AXIS2_PLACEMENT_3D ( 'NONE', #13129, #8415, #2671 ) ;
#7510 = CARTESIAN_POINT ( 'NONE',  ( 1.000000000000000222, -0.4429999999999998939, 0.5000000000000000000 ) ) ;
#7511 = FACE_OUTER_BOUND ( 'NONE', #5831, .T. ) ;
#7512 = VERTEX_POINT ( 'NONE', #6374 ) ;
#7513 = CARTESIAN_POINT ( 'NONE',  ( 6.215861650065340527, 0.000000000000000000, 0.000000000000000000 ) ) ;
#7514 = ORIENTED_EDGE ( 'NONE', *, *, #2286, .F. ) ;
#7515 = DIRECTION ( 'NONE',  ( 0.000000000000000000, 0.000000000000000000, 1.000000000000000000 ) ) ;
#7516 = CARTESIAN_POINT ( 'NONE',  ( 1.250000000000000000, 0.000000000000000000, -0.4223386481965726302 ) ) ;
#7517 = AXIS2_PLACEMENT_3D ( 'NONE', #7948, #3437, #3210 ) ;
#7518 = CARTESIAN_POINT ( 'NONE',  ( 0.7818165671723676935, -0.4451953551292709421, -0.3317768536406905944 ) ) ;
#7519 = CARTESIAN_POINT ( 'NONE',  ( 6.208491571325183145, 1.679378605318035733, -1.304378605318064821 ) ) ;
#7520 = DIRECTION ( 'NONE',  ( 0.000000000000000000, 0.000000000000000000, -1.000000000000000000 ) ) ;
#7521 = ADVANCED_FACE ( 'NONE', ( #9737 ), #2083, .F. ) ;
#7522 = CARTESIAN_POINT ( 'NONE',  ( 1.323631913064688748, -9.281535253675872034E-17, -0.4212431828231353870 ) ) ;
#7523 = AXIS2_PLACEMENT_3D ( 'NONE', #12795, #11664, #460 ) ;
#7524 = CARTESIAN_POINT ( 'NONE',  ( 6.794491571325179891, -1.679378605318047946, -1.679378605318053497 ) ) ;
#7525 = ORIENTED_EDGE ( 'NONE', *, *, #7205, .F. ) ;
#7526 = ORIENTED_EDGE ( 'NONE', *, *, #9833, .F. ) ;
#7527 = EDGE_LOOP ( 'NONE', ( #1837, #11194, #7492, #3183 ) ) ;
#7528 = CARTESIAN_POINT ( 'NONE',  ( 8.573547510565946439, 0.9318103594814406421, -0.3691840008912834481 ) ) ;
#7529 = ORIENTED_EDGE ( 'NONE', *, *, #2265, .F. ) ;
#7530 = CARTESIAN_POINT ( 'NONE',  ( 2.814370078740158210, 1.224646799147353207E-16, -1.000000000000000000 ) ) ;
#7531 = DIRECTION ( 'NONE',  ( 0.000000000000000000, 0.000000000000000000, 1.000000000000000000 ) ) ;
#7532 = CIRCLE ( 'NONE', #1897, 0.4070000000000046914 ) ;
#7533 = LINE ( 'NONE', #473, #8786 ) ;
#7534 = AXIS2_PLACEMENT_3D ( 'NONE', #739, #7501, #6504 ) ;
#7535 = CARTESIAN_POINT ( 'NONE',  ( 4.620520747435304720, 1.809297920034194984, -0.09820618556490041950 ) ) ;
#7536 = EDGE_CURVE ( 'NONE', #4996, #13246, #8687, .T. ) ;
#7537 = ADVANCED_FACE ( 'NONE', ( #11026 ), #12096, .T. ) ;
#7538 = EDGE_CURVE ( 'NONE', #10975, #11724, #6991, .T. ) ;
#7539 = CARTESIAN_POINT ( 'NONE',  ( -0.4125000000000001998, -0.6590000000000000302, -0.4125000000000000333 ) ) ;
#7540 = CIRCLE ( 'NONE', #1189, 0.03999999999999998002 ) ;
#7541 = AXIS2_PLACEMENT_3D ( 'NONE', #7581, #12240, #7507 ) ;
#7542 = CIRCLE ( 'NONE', #10235, 0.7500000000000001110 ) ;
#7543 = ORIENTED_EDGE ( 'NONE', *, *, #546, .T. ) ;
#7544 = VERTEX_POINT ( 'NONE', #11173 ) ;
#7545 = ADVANCED_FACE ( 'NONE', ( #4067 ), #6297, .F. ) ;
#7546 = AXIS2_PLACEMENT_3D ( 'NONE', #4035, #9847, #6639 ) ;
#7547 = EDGE_LOOP ( 'NONE', ( #11464, #7855, #1586, #13757 ) ) ;
#7548 = CARTESIAN_POINT ( 'NONE',  ( 0.3725000000000000533, 0.1749999999999999889, 0.4124999999999999778 ) ) ;
#7549 = CARTESIAN_POINT ( 'NONE',  ( 4.271631709730848492, 0.9523919498644370929, 0.3061575615593492561 ) ) ;
#7550 = LINE ( 'NONE', #8625, #14605 ) ;
#7551 = VERTEX_POINT ( 'NONE', #13381 ) ;
#7552 = LINE ( 'NONE', #4108, #9227 ) ;
#7553 = FACE_OUTER_BOUND ( 'NONE', #11294, .T. ) ;
#7554 = CARTESIAN_POINT ( 'NONE',  ( 2.326828918379972104E-17, 0.000000000000000000, 0.1900000000000000577 ) ) ;
#7555 = PRESENTATION_LAYER_ASSIGNMENT (  '', '', ( #15123 ) ) ;
#7556 = ADVANCED_FACE ( 'NONE', ( #2925 ), #11129, .T. ) ;
#7557 = VECTOR ( 'NONE', #5717, 39.37007874015748143 ) ;
#7558 = CARTESIAN_POINT ( 'NONE',  ( 8.792093969802149189, 0.8799778768672790186, 6.829619984160658046E-17 ) ) ;
#7559 = DIRECTION ( 'NONE',  ( 1.000000000000000000, 0.000000000000000000, 0.000000000000000000 ) ) ;
#7560 = CARTESIAN_POINT ( 'NONE',  ( 2.774999999999999911, -1.679378605318059048, -1.679378605318041950 ) ) ;
#7561 = CARTESIAN_POINT ( 'NONE',  ( 3.874999999999999556, 2.750000000000000000, -1.320000000000000062 ) ) ;
#7563 = ORIENTED_EDGE ( 'NONE', *, *, #5141, .F. ) ;
#7562 = LINE ( 'NONE', #1585, #7675 ) ;
#7564 = ORIENTED_EDGE ( 'NONE', *, *, #9280, .F. ) ;
#7565 = CARTESIAN_POINT ( 'NONE',  ( -0.2936128187763769604, 1.600826314462298283, -0.2533531860778197031 ) ) ;
#7567 = VERTEX_POINT ( 'NONE', #5289 ) ;
#7566 = DIRECTION ( 'NONE',  ( 0.000000000000000000, 0.000000000000000000, 1.000000000000000000 ) ) ;
#7568 = ORIENTED_EDGE ( 'NONE', *, *, #1453, .F. ) ;
#7569 = EDGE_CURVE ( 'NONE', #3205, #287, #7719, .T. ) ;
#7570 = VECTOR ( 'NONE', #4159, 39.37007874015748143 ) ;
#7571 = CARTESIAN_POINT ( 'NONE',  ( 3.063895178286539789, 1.056999999999999718, -0.3964908961568774926 ) ) ;
#7572 =( LENGTH_UNIT ( ) NAMED_UNIT ( * ) SI_UNIT ( $, .METRE. ) );
#7573 = CARTESIAN_POINT ( 'NONE',  ( 3.426491571325181340, 1.679378605318042395, -1.973878605318056367 ) ) ;
#7574 = ORIENTED_EDGE ( 'NONE', *, *, #9048, .T. ) ;
#7575 = DIRECTION ( 'NONE',  ( -0.000000000000000000, -1.000000000000000000, -0.000000000000000000 ) ) ;
#7576 = DIRECTION ( 'NONE',  ( 0.8970266063945135926, 0.000000000000000000, -0.4419765462333294370 ) ) ;
#7577 = ADVANCED_FACE ( 'NONE', ( #7511 ), #1688, .F. ) ;
#7578 = CARTESIAN_POINT ( 'NONE',  ( 0.6894988814560862878, -0.0004723380455460435431, 0.4465617225471406049 ) ) ;
#7579 = CARTESIAN_POINT ( 'NONE',  ( 0.9699525753244386816, -0.4431216144847617833, -0.4027229741727945678 ) ) ;
#7580 = EDGE_LOOP ( 'NONE', ( #11559, #5433, #12075, #2139 ) ) ;
#7581 = CARTESIAN_POINT ( 'NONE',  ( 6.176491571325181340, -1.679378605318047946, -1.679378605318053497 ) ) ;
#7582 = DIRECTION ( 'NONE',  ( -0.9992912762382415437, -0.03489602031261516274, -0.01411428356269072565 ) ) ;
#7583 = FACE_OUTER_BOUND ( 'NONE', #4808, .T. ) ;
#7584 = ORIENTED_EDGE ( 'NONE', *, *, #7198, .T. ) ;
#7585 = CARTESIAN_POINT ( 'NONE',  ( 4.007132756949598473, 0.8754566745458228771, -0.4833557680116081778 ) ) ;
#7586 = LINE ( 'NONE', #5377, #11623 ) ;
#7587 = ORIENTED_EDGE ( 'NONE', *, *, #2250, .F. ) ;
#7588 = CARTESIAN_POINT ( 'NONE',  ( -0.4313007445438682974, 1.564783867144732277, 0.01487070305975445560 ) ) ;
#7589 = ORIENTED_EDGE ( 'NONE', *, *, #3252, .T. ) ;
#7590 = CARTESIAN_POINT ( 'NONE',  ( 3.874999999999999556, 3.137999999999999901, 1.320000000000000062 ) ) ;
#7591 = EDGE_CURVE ( 'NONE', #9235, #754, #13457, .T. ) ;
#7592 = EDGE_CURVE ( 'NONE', #8434, #4931, #14064, .T. ) ;
#7593 = DIRECTION ( 'NONE',  ( 0.9999002670844989726, 1.365787769249574676E-16, -0.01412288512831212997 ) ) ;
#7594 = DIRECTION ( 'NONE',  ( -0.000000000000000000, -1.000000000000000000, -0.000000000000000000 ) ) ;
#7595 = DIRECTION ( 'NONE',  ( -0.7071067811865376918, 8.659560562355053653E-17, -0.7071067811865573427 ) ) ;
#7596 = DIRECTION ( 'NONE',  ( -0.000000000000000000, -1.000000000000000000, -0.000000000000000000 ) ) ;
#7597 = CARTESIAN_POINT ( 'NONE',  ( 1.558097216777239780, -0.02209972869556142000, -0.4779929771641632796 ) ) ;
#7598 = CARTESIAN_POINT ( 'NONE',  ( 3.426491571325181340, -1.679378605318041950, 1.679378605318059048 ) ) ;
#7599 = ORIENTED_EDGE ( 'NONE', *, *, #3684, .T. ) ;
#7600 = ORIENTED_EDGE ( 'NONE', *, *, #9706, .T. ) ;
#7601 = VERTEX_POINT ( 'NONE', #8886 ) ;
#7602 = CARTESIAN_POINT ( 'NONE',  ( 8.575402687748473696, 0.8724108505558056947, -0.3686609533457590460 ) ) ;
#7603 = EDGE_LOOP ( 'NONE', ( #1495, #9173, #14621, #2627 ) ) ;
#7604 = LINE ( 'NONE', #12265, #14521 ) ;
#7605 = FACE_OUTER_BOUND ( 'NONE', #15095, .T. ) ;
#7606 = EDGE_CURVE ( 'NONE', #3928, #7512, #3073, .T. ) ;
#7607 = VECTOR ( 'NONE', #13333, 39.37007874015748143 ) ;
#7608 = DIRECTION ( 'NONE',  ( -0.000000000000000000, 0.000000000000000000, 1.000000000000000000 ) ) ;
#7609 = CARTESIAN_POINT ( 'NONE',  ( 4.626583745745669773, 1.810565237260122418, -0.02390113810800691824 ) ) ;
#7610 = ORIENTED_EDGE ( 'NONE', *, *, #8453, .T. ) ;
#7611 = ORIENTED_EDGE ( 'NONE', *, *, #8686, .F. ) ;
#7612 = VERTEX_POINT ( 'NONE', #6831 ) ;
#7613 = ORIENTED_EDGE ( 'NONE', *, *, #6068, .F. ) ;
#7614 = B_SPLINE_CURVE_WITH_KNOTS ( 'NONE', 3,
 ( #4220, #2135, #11400, #13526, #9189, #6828, #10330, #14992, #8882, #3068, #7735, #12390, #1906, #6594, #5444, #10110, #14763, #2604, #11785, #12924, #4908, #9574, #5904, #9347, #14218, #13985, #2292, #8202, #8360, #1285, #11858, #10634, #1214, #1135, #5827, #12842, #8283, #1359, #12764, #206, #3448, #7204, #10560, #4676, #2375, #10489, #3521, #11555, #1057, #5745, #10411, #15073, #3682, #6049, #12993, #7054 ),
 .UNSPECIFIED., .F., .F.,
 ( 4, 2, 2, 2, 2, 2, 2, 2, 2, 2, 2, 2, 2, 2, 2, 2, 2, 2, 2, 2, 2, 2, 2, 2, 2, 2, 2, 4 ),
 ( 0.000000000000000000, 0.001913177148301513928, 0.003826354296603027855, 0.005739531444904541133, 0.007652708593206055711, 0.01147906288980911349, 0.01339224003811062894, 0.01530541718641214612, 0.01913177148301517527, 0.02104494863131669072, 0.02295812577961820616, 0.02678448007622125787, 0.02774106865037202080, 0.02869765722452279066, 0.03061083437282431305, 0.03443718866942736129, 0.03539377724357812421, 0.03635036581772889408, 0.03826354296603043381, 0.04208989726263349940, 0.04400307441093503219, 0.04591625155923656498, 0.04782942870753809778, 0.04974260585583962363, 0.05356896015244266840, 0.05548213730074420813, 0.05739531444904575480, 0.06122166874564884120 ),
 .UNSPECIFIED. ) ;
#7615 = DIRECTION ( 'NONE',  ( 0.01412288512831213171, -3.675428035873182550E-19, 0.9999002670844991947 ) ) ;
#7616 = ADVANCED_FACE ( 'NONE', ( #9192 ), #13805, .F. ) ;
#7617 = DIRECTION ( 'NONE',  ( 0.000000000000000000, 0.000000000000000000, -1.000000000000000000 ) ) ;
#7618 = CARTESIAN_POINT ( 'NONE',  ( 3.958015244391202447, 0.8698464393224263347, 0.4933369105775312069 ) ) ;
#7619 = CONTEXT_DEPENDENT_SHAPE_REPRESENTATION ( #9978, #3725 ) ;
#7620 = CARTESIAN_POINT ( 'NONE',  ( 2.599116034106475404, 0.7926631980420985046, 0.4028586330191923914 ) ) ;
#7621 =( REPRESENTATION_RELATIONSHIP ('NONE','NONE', #3591, #8297 ) REPRESENTATION_RELATIONSHIP_WITH_TRANSFORMATION ( #12209 )SHAPE_REPRESENTATION_RELATIONSHIP( ) );
#7622 = VERTEX_POINT ( 'NONE', #11404 ) ;
#7623 = CARTESIAN_POINT ( 'NONE',  ( 2.774999999999999911, 0.9799999999999436939, -3.360000000000016751 ) ) ;
#7624 = DIRECTION ( 'NONE',  ( -0.9396926207859107594, 0.000000000000000000, 0.3420201433256624401 ) ) ;
#7625 = LINE ( 'NONE', #3963, #9283 ) ;
#7626 = PRODUCT_DEFINITION_SHAPE ( 'NONE', 'NONE',  #13772 ) ;
#7627 = CARTESIAN_POINT ( 'NONE',  ( 8.803302564019910292, 0.8803692896022998760, 0.1890918720381998541 ) ) ;
#7628 = CARTESIAN_POINT ( 'NONE',  ( 0.9492541663682917408, -0.4468142390482141568, -0.4325038486745500510 ) ) ;
#7629 = CARTESIAN_POINT ( 'NONE',  ( 3.893742162958262032, 1.774205514365693181, 0.7983174907408143728 ) ) ;
#7631 = ORIENTED_EDGE ( 'NONE', *, *, #2413, .F. ) ;
#7630 = FACE_OUTER_BOUND ( 'NONE', #5308, .T. ) ;
#7632 = AXIS2_PLACEMENT_3D ( 'NONE', #14459, #13374, #8655 ) ;
#7633 = EDGE_LOOP ( 'NONE', ( #8816, #1782, #6997, #311 ) ) ;
#7634 = CARTESIAN_POINT ( 'NONE',  ( -0.4192535942842267049, 1.577705975193670840, -0.03573697939586736871 ) ) ;
#7636 = EDGE_LOOP ( 'NONE', ( #2271, #12801, #8181, #3988 ) ) ;
#7635 = DIRECTION ( 'NONE',  ( -1.000000000000000000, -0.000000000000000000, -0.000000000000000000 ) ) ;
#7637 = EDGE_LOOP ( 'NONE', ( #14103, #7433, #4328, #13016, #10860 ) ) ;
#7638 = EDGE_CURVE ( 'NONE', #3117, #14571, #1910, .T. ) ;
#7639 = EDGE_CURVE ( 'NONE', #13316, #6459, #3373, .T. ) ;
#7640 = CARTESIAN_POINT ( 'NONE',  ( 0.000000000000000000, 1.159999999999999698, -0.1899999999999999745 ) ) ;
#7641 = SHAPE_REPRESENTATION_RELATIONSHIP ( 'NONE' , 'NONE' ,  #2091, #3279 ) ;
#7642 = CARTESIAN_POINT ( 'NONE',  ( 8.849999999999999645, 0.9399413264884247665, 6.829619984160658046E-17 ) ) ;
#7643 = VERTEX_POINT ( 'NONE', #10332 ) ;
#7644 = ADVANCED_FACE ( 'NONE', ( #13686 ), #5747, .F. ) ;
#7645 = LINE ( 'NONE', #3055, #3313 ) ;
#7646 = DIRECTION ( 'NONE',  ( -1.000000000000000000, -0.000000000000000000, -0.000000000000000000 ) ) ;
#7647 = ADVANCED_FACE ( 'NONE', ( #12699 ), #1060, .T. ) ;
#7648 = LINE ( 'NONE', #9729, #3060 ) ;
#7649 = DIRECTION ( 'NONE',  ( 0.000000000000000000, 1.000000000000000000, 0.000000000000000000 ) ) ;
#7650 = EDGE_CURVE ( 'NONE', #5634, #6979, #12616, .T. ) ;
#7651 = ORIENTED_EDGE ( 'NONE', *, *, #9887, .F. ) ;
#7652 = CARTESIAN_POINT ( 'NONE',  ( 3.426491571325181340, 1.679378605318042395, -1.384878605318061062 ) ) ;
#7653 = CIRCLE ( 'NONE', #12051, 0.8653656741516848605 ) ;
#7654 = CARTESIAN_POINT ( 'NONE',  ( 2.527624975756972425, 2.750000000000000000, 0.9199802545633498640 ) ) ;
#7655 = DIRECTION ( 'NONE',  ( 1.000000000000000000, 0.000000000000000000, 0.000000000000000000 ) ) ;
#7656 = CIRCLE ( 'NONE', #5721, 0.7435009325572419225 ) ;
#7657 = VERTEX_POINT ( 'NONE', #751 ) ;
#7658 = CARTESIAN_POINT ( 'NONE',  ( 4.205440198960407550, 0.9266839483850188852, -0.3766322587779434850 ) ) ;
#7659 = DIRECTION ( 'NONE',  ( 0.000000000000000000, 0.000000000000000000, -1.000000000000000000 ) ) ;
#7660 = ORIENTED_EDGE ( 'NONE', *, *, #4943, .T. ) ;
#7661 = FACE_OUTER_BOUND ( 'NONE', #4534, .T. ) ;
#7662 = FACE_OUTER_BOUND ( 'NONE', #12191, .T. ) ;
#7663 = LINE ( 'NONE', #10889, #2192 ) ;
#7664 = EDGE_CURVE ( 'NONE', #12484, #7097, #982, .T. ) ;
#7665 = CONICAL_SURFACE ( 'NONE', #7908, 0.2944999999999998175, 0.7853981633974530530 ) ;
#7666 = CARTESIAN_POINT ( 'NONE',  ( 1.519298119451261364, -0.3788322150377887443, 0.4785409870134300636 ) ) ;
#7667 = LINE ( 'NONE', #8534, #2879 ) ;
#7668 = FACE_BOUND ( 'NONE', #14224, .T. ) ;
#7669 = ADVANCED_FACE ( 'NONE', ( #5603 ), #12115, .F. ) ;
#7670 = VERTEX_POINT ( 'NONE', #10415 ) ;
#7671 = LINE ( 'NONE', #3170, #10387 ) ;
#7672 = CARTESIAN_POINT ( 'NONE',  ( 1.249999999999997335, 9.390727478220904197E-17, -0.4223386481965728523 ) ) ;
#7673 = EDGE_CURVE ( 'NONE', #9005, #11004, #9043, .T. ) ;
#7674 =( NAMED_UNIT ( * ) PLANE_ANGLE_UNIT ( ) SI_UNIT ( $, .RADIAN. ) );
#7675 = VECTOR ( 'NONE', #2821, 39.37007874015748854 ) ;
#7676 = DIRECTION ( 'NONE',  ( -1.000000000000000000, -0.000000000000000000, -0.000000000000000000 ) ) ;
#7677 = ORIENTED_EDGE ( 'NONE', *, *, #6098, .F. ) ;
#7678 = VERTEX_POINT ( 'NONE', #10266 ) ;
#7679 = VECTOR ( 'NONE', #12620, 39.37007874015748143 ) ;
#7680 = CARTESIAN_POINT ( 'NONE',  ( 3.426491571325181340, -3.000039370078740220, -0.5999481385559802815 ) ) ;
#7681 = ORIENTED_EDGE ( 'NONE', *, *, #1437, .F. ) ;
#7682 = DIRECTION ( 'NONE',  ( 0.000000000000000000, 0.000000000000000000, -1.000000000000000000 ) ) ;
#7683 = CARTESIAN_POINT ( 'NONE',  ( 0.6592137334438913365, -0.4436300111355807596, -0.4885243083254872110 ) ) ;
#7684 = CARTESIAN_POINT ( 'NONE',  ( 3.426491571325181340, 2.015586091437299388, -0.6121388925861622754 ) ) ;
#7685 = AXIS2_PLACEMENT_3D ( 'NONE', #8836, #9065, #3242 ) ;
#7686 = DIRECTION ( 'NONE',  ( -1.000000000000000000, -0.000000000000000000, -0.000000000000000000 ) ) ;
#7687 = EDGE_LOOP ( 'NONE', ( #943, #13542, #11868, #12786 ) ) ;
#7688 = EDGE_CURVE ( 'NONE', #6864, #4931, #11255, .T. ) ;
#7689 = CARTESIAN_POINT ( 'NONE',  ( 4.198116201031909078, 1.736978055819331512, -0.6778351007205051237 ) ) ;
#7690 = VERTEX_POINT ( 'NONE', #11326 ) ;
#7691 = EDGE_LOOP ( 'NONE', ( #3592, #2261 ) ) ;
#7692 = AXIS2_PLACEMENT_3D ( 'NONE', #9774, #9925, #13342 ) ;
#7693 = ORIENTED_EDGE ( 'NONE', *, *, #9491, .T. ) ;
#7694 = CARTESIAN_POINT ( 'NONE',  ( 8.476283996537762988, 0.8689495495877206377, 0.3203020658980471613 ) ) ;
#7695 = CIRCLE ( 'NONE', #583, 0.4070000000000025264 ) ;
#7696 = VECTOR ( 'NONE', #12237, 39.37007874015748143 ) ;
#7697 = CARTESIAN_POINT ( 'NONE',  ( 2.774999999999999911, 1.679378605318042395, -1.941878605318058115 ) ) ;
#7698 = CARTESIAN_POINT ( 'NONE',  ( 4.375014056583601096, 1.000007028289835675, -0.01611911748198105107 ) ) ;
#7699 = ITEM_DEFINED_TRANSFORMATION ( 'NONE', 'NONE', #5476,  #8424 ) ;
#7700 = CARTESIAN_POINT ( 'NONE',  ( 0.1787546228633458134, 1.577672892097735202, -0.3809527529760087239 ) ) ;
#7701 = EDGE_LOOP ( 'NONE', ( #11648, #7232 ) ) ;
#7702 = DIRECTION ( 'NONE',  ( 0.000000000000000000, 1.000000000000000000, 0.000000000000000000 ) ) ;
#7703 = LINE ( 'NONE', #4109, #5344 ) ;
#7704 = CARTESIAN_POINT ( 'NONE',  ( 3.876560711617219379, 1.855806856933289950, 0.7500000000000001110 ) ) ;
#7705 = CARTESIAN_POINT ( 'NONE',  ( 8.476283996537762988, 0.8689495495877206377, -0.3203020658980470503 ) ) ;
#7706 = CARTESIAN_POINT ( 'NONE',  ( 8.670688874134258484, 0.8757383175063380154, 0.2544954840226653636 ) ) ;
#7707 = VECTOR ( 'NONE', #7803, 39.37007874015748143 ) ;
#7708 = CIRCLE ( 'NONE', #14782, 0.07999999999999996003 ) ;
#7709 = CARTESIAN_POINT ( 'NONE',  ( 0.8902005033493116670, -0.4418901924079376431, -0.4498168137707627690 ) ) ;
#7710 = ADVANCED_FACE ( 'NONE', ( #9277, #13915, #7738, #4521, #2222, #6904 ), #4601, .F. ) ;
#7711 = CARTESIAN_POINT ( 'NONE',  ( 3.836102718394629019, 1.791032951870848544, 0.7985211043516597940 ) ) ;
#7713 = ORIENTED_EDGE ( 'NONE', *, *, #2012, .F. ) ;
#7712 = CARTESIAN_POINT ( 'NONE',  ( 3.631360142079332665, 1.967959863695790457, -0.4367743950684919718 ) ) ;
#7714 = VERTEX_POINT ( 'NONE', #13756 ) ;
#7716 = EDGE_LOOP ( 'NONE', ( #6440, #7943, #11, #4189 ) ) ;
#7715 = DIRECTION ( 'NONE',  ( -0.000000000000000000, -1.000000000000000000, -0.000000000000000000 ) ) ;
#7717 = ORIENTED_EDGE ( 'NONE', *, *, #14185, .T. ) ;
#7718 = DIRECTION ( 'NONE',  ( -0.000000000000000000, -1.000000000000000000, -0.000000000000000000 ) ) ;
#7719 = CIRCLE ( 'NONE', #10413, 0.9499999999999988454 ) ;
#7720 =( NAMED_UNIT ( * ) PLANE_ANGLE_UNIT ( ) SI_UNIT ( $, .RADIAN. ) );
#7721 = CARTESIAN_POINT ( 'NONE',  ( 0.1807106342563528367, 1.379999999999999671, 5.178337979384803075E-18 ) ) ;
#7722 = ORIENTED_EDGE ( 'NONE', *, *, #2045, .T. ) ;
#7723 = DIRECTION ( 'NONE',  ( 0.7071067811865430208, -0.7071067811865520136, 0.000000000000000000 ) ) ;
#7724 = CARTESIAN_POINT ( 'NONE',  ( 0.3724999999999997757, 0.2159999999999999420, -0.3725000000000000533 ) ) ;
#7725 = CIRCLE ( 'NONE', #371, 1.409999999999999920 ) ;
#7726 = CARTESIAN_POINT ( 'NONE',  ( 2.742551415177088003, 0.8007359432430825041, -0.4612633980907191456 ) ) ;
#7727 = EDGE_CURVE ( 'NONE', #1043, #9581, #1109, .T. ) ;
#7728 = DIRECTION ( 'NONE',  ( 0.000000000000000000, 1.000000000000000000, 0.000000000000000000 ) ) ;
#7729 = EDGE_CURVE ( 'NONE', #9809, #1024, #2090, .T. ) ;
#7730 = ORIENTED_EDGE ( 'NONE', *, *, #6693, .T. ) ;
#7731 = AXIS2_PLACEMENT_3D ( 'NONE', #6724, #9026, #8028 ) ;
#7732 = ADVANCED_FACE ( 'NONE', ( #7816 ), #7977, .F. ) ;
#7733 = DIRECTION ( 'NONE',  ( -0.000000000000000000, -1.000000000000000000, -0.000000000000000000 ) ) ;
#7734 = DIRECTION ( 'NONE',  ( 0.3420201433256620516, 0.000000000000000000, 0.9396926207859108704 ) ) ;
#7735 = CARTESIAN_POINT ( 'NONE',  ( 4.313738930246985070, 1.707933241827553683, -0.6660024015622548754 ) ) ;
#7736 = EDGE_LOOP ( 'NONE', ( #6982, #6684 ) ) ;
#7737 = CARTESIAN_POINT ( 'NONE',  ( 0.7007544714965477928, -0.4010719056816615113, 0.4875120335496959667 ) ) ;
#7738 = FACE_BOUND ( 'NONE', #9025, .T. ) ;
#7739 = EDGE_LOOP ( 'NONE', ( #3969, #5676 ) ) ;
#7740 = EDGE_CURVE ( 'NONE', #7304, #282, #7482, .T. ) ;
#7741 = DIRECTION ( 'NONE',  ( -1.000000000000000000, -0.000000000000000000, -0.000000000000000000 ) ) ;
#7742 = ORIENTED_EDGE ( 'NONE', *, *, #12642, .T. ) ;
#7743 = AXIS2_PLACEMENT_3D ( 'NONE', #11444, #6702, #6475 ) ;
#7744 = LINE ( 'NONE', #1839, #13662 ) ;
#7745 = LENGTH_MEASURE_WITH_UNIT ( LENGTH_MEASURE( 0.02539999999999999897 ), #1922 );
#7746 = DIRECTION ( 'NONE',  ( 1.000000000000000000, 0.000000000000000000, 0.000000000000000000 ) ) ;
#7747 = DIRECTION ( 'NONE',  ( -0.000000000000000000, -1.000000000000000000, -0.000000000000000000 ) ) ;
#7748 = ORIENTED_EDGE ( 'NONE', *, *, #9380, .T. ) ;
#7749 = CARTESIAN_POINT ( 'NONE',  ( 4.344846310392954436, 3.137999999999999901, 1.491010071662831393 ) ) ;
#7750 = CARTESIAN_POINT ( 'NONE',  ( 0.8321296539245407464, -0.4837347236987069587, -0.3428806532137185226 ) ) ;
#7751 = CARTESIAN_POINT ( 'NONE',  ( 0.4349147617188415249, 1.239999999999999991, 0.008611041693268213504 ) ) ;
#7752 = VECTOR ( 'NONE', #5711, 39.37007874015748143 ) ;
#7753 = CARTESIAN_POINT ( 'NONE',  ( 3.876560711617219379, -3.000039370078740220, 0.000000000000000000 ) ) ;
#7754 = ORIENTED_EDGE ( 'NONE', *, *, #2021, .T. ) ;
#7755 = ORIENTED_EDGE ( 'NONE', *, *, #2103, .F. ) ;
#7756 = CARTESIAN_POINT ( 'NONE',  ( 3.874999999999999556, 3.137999999999999901, -1.320000000000000062 ) ) ;
#7757 = ORIENTED_EDGE ( 'NONE', *, *, #2447, .T. ) ;
#7758 = CARTESIAN_POINT ( 'NONE',  ( 3.944129661530210385, 0.000000000000000000, 0.000000000000000000 ) ) ;
#7759 = CONICAL_SURFACE ( 'NONE', #6055, 0.3750000000000004996, 0.7853981633974557175 ) ;
#7760 = EDGE_CURVE ( 'NONE', #4263, #5088, #1444, .T. ) ;
#7761 = FACE_OUTER_BOUND ( 'NONE', #5290, .T. ) ;
#7762 = CARTESIAN_POINT ( 'NONE',  ( 0.8999999999999998002, 0.000000000000000000, -0.2749999999999998557 ) ) ;
#7763 = EDGE_CURVE ( 'NONE', #6255, #4759, #9648, .T. ) ;
#7764 = CARTESIAN_POINT ( 'NONE',  ( 0.000000000000000000, 4.529999999999999361, 0.000000000000000000 ) ) ;
#7765 = AXIS2_PLACEMENT_3D ( 'NONE', #1241, #8457, #6157 ) ;
#7766 = ORIENTED_EDGE ( 'NONE', *, *, #4370, .T. ) ;
#7767 = DIRECTION ( 'NONE',  ( 0.000000000000000000, 0.000000000000000000, 1.000000000000000000 ) ) ;
#7768 = AXIS2_PLACEMENT_3D ( 'NONE', #1735, #14374, #2829 ) ;
#7769 = CARTESIAN_POINT ( 'NONE',  ( 4.233629482522627718, 1.713288744528204788, -0.7097370609146418374 ) ) ;
#7770 = ORIENTED_EDGE ( 'NONE', *, *, #5314, .T. ) ;
#7771 = ORIENTED_EDGE ( 'NONE', *, *, #7425, .T. ) ;
#7772 = ORIENTED_EDGE ( 'NONE', *, *, #4030, .F. ) ;
#7773 = AXIS2_PLACEMENT_3D ( 'NONE', #5042, #12140, #14494 ) ;
#7774 = DIRECTION ( 'NONE',  ( 0.000000000000000000, 1.000000000000000000, -0.000000000000000000 ) ) ;
#7775 = DIRECTION ( 'NONE',  ( 0.000000000000000000, 1.000000000000000000, 0.000000000000000000 ) ) ;
#7777 = FACE_OUTER_BOUND ( 'NONE', #14790, .T. ) ;
#7776 = CIRCLE ( 'NONE', #1166, 0.05999999999999990757 ) ;
#7778 = CARTESIAN_POINT ( 'NONE',  ( 0.2027934381167127154, 1.564766993392023631, -0.3809527529760087239 ) ) ;
#7779 = ORIENTED_EDGE ( 'NONE', *, *, #2625, .F. ) ;
#7780 = DIRECTION ( 'NONE',  ( -1.000000000000000000, -0.000000000000000000, -0.000000000000000000 ) ) ;
#7781 = DIRECTION ( 'NONE',  ( 1.000000000000000000, 0.000000000000000000, 0.000000000000000000 ) ) ;
#7782 = EDGE_CURVE ( 'NONE', #12826, #11117, #10791, .T. ) ;
#7783 = ADVANCED_FACE ( 'NONE', ( #1289 ), #10713, .F. ) ;
#7784 = CARTESIAN_POINT ( 'NONE',  ( -0.4124999999999999223, 0.000000000000000000, -0.4124999999999999778 ) ) ;
#7785 = DIRECTION ( 'NONE',  ( 0.000000000000000000, 1.000000000000000000, 0.000000000000000000 ) ) ;
#7786 = AXIS2_PLACEMENT_3D ( 'NONE', #3085, #9972, #4390 ) ;
#7787 = CIRCLE ( 'NONE', #8039, 0.03999999999999998002 ) ;
#7788 = PRESENTATION_LAYER_ASSIGNMENT (  '', '', ( #10969 ) ) ;
#7789 = AXIS2_PLACEMENT_3D ( 'NONE', #11222, #5120, #6483 ) ;
#7790 = CARTESIAN_POINT ( 'NONE',  ( 0.9387684931985510461, -0.4323728853731128030, -0.4608802220936111804 ) ) ;
#7791 = AXIS2_PLACEMENT_3D ( 'NONE', #8784, #5338, #8857 ) ;
#7792 = CARTESIAN_POINT ( 'NONE',  ( 4.159006841833645218, 1.720943226083167188, 0.7430362912831911526 ) ) ;
#7794 = ORIENTED_EDGE ( 'NONE', *, *, #6098, .T. ) ;
#7793 = LINE ( 'NONE', #14820, #13280 ) ;
#7795 = VERTEX_POINT ( 'NONE', #8427 ) ;
#7797 = EDGE_LOOP ( 'NONE', ( #8478, #14891, #10674, #1621 ) ) ;
#7796 = CARTESIAN_POINT ( 'NONE',  ( 3.875000000000000000, 1.112678268764263789, 0.000000000000000000 ) ) ;
#7798 = CONICAL_SURFACE ( 'NONE', #1429, 0.08500000000000004774, 0.7853981633974541632 ) ;
#7799 = ORIENTED_EDGE ( 'NONE', *, *, #7147, .T. ) ;
#7800 = CARTESIAN_POINT ( 'NONE',  ( 0.4125000000000000333, 0.1749999999999999889, -0.4124999999999999778 ) ) ;
#7801 = CARTESIAN_POINT ( 'NONE',  ( 3.426491571325181340, 0.000000000000000000, 0.000000000000000000 ) ) ;
#7802 = ORIENTED_EDGE ( 'NONE', *, *, #995, .T. ) ;
#7803 = DIRECTION ( 'NONE',  ( -0.000000000000000000, -1.000000000000000000, -0.000000000000000000 ) ) ;
#7804 = DIRECTION ( 'NONE',  ( 0.4419764427789427685, 0.0006842106276663988736, 0.8970263964255951183 ) ) ;
#7805 = CIRCLE ( 'NONE', #4887, 0.7849999999999996980 ) ;
#7806 = CARTESIAN_POINT ( 'NONE',  ( 3.426491571325181340, -1.679378605318059048, -1.679378605318041950 ) ) ;
#7807 = CARTESIAN_POINT ( 'NONE',  ( 2.630032447663877893, 0.7405933021012496287, -0.4628526490442955166 ) ) ;
#7808 = CARTESIAN_POINT ( 'NONE',  ( 1.014070859989637308, -0.4429514566285153720, -0.3903639285911673640 ) ) ;
#7809 = ORIENTED_EDGE ( 'NONE', *, *, #1714, .F. ) ;
#7810 = CONICAL_SURFACE ( 'NONE', #1203, 0.1050000000000001071, 0.7853981633974560506 ) ;
#7811 = CARTESIAN_POINT ( 'NONE',  ( 0.4529333289293680509, 0.1749999999999999889, -1.690370196005881009 ) ) ;
#7812 = CARTESIAN_POINT ( 'NONE',  ( 3.623103638349538524, 0.9015510240917827822, -0.4331298522267356677 ) ) ;
#7813 = DIRECTION ( 'NONE',  ( 0.7071067811865501263, 0.000000000000000000, -0.7071067811865449082 ) ) ;
#7814 = CONICAL_SURFACE ( 'NONE', #4903, 0.3750000000000004996, 0.7853981633974547183 ) ;
#7815 = CYLINDRICAL_SURFACE ( 'NONE', #3807, 1.000000000000000222 ) ;
#7816 = FACE_OUTER_BOUND ( 'NONE', #10417, .T. ) ;
#7817 = ORIENTED_EDGE ( 'NONE', *, *, #2533, .F. ) ;
#7818 = CARTESIAN_POINT ( 'NONE',  ( 0.9652173913043479159, -0.4829999999999998739, -0.3379636412230419551 ) ) ;
#7819 = ORIENTED_EDGE ( 'NONE', *, *, #3518, .T. ) ;
#7820 = ADVANCED_FACE ( 'NONE', ( #9502 ), #14067, .F. ) ;
#7821 = AXIS2_PLACEMENT_3D ( 'NONE', #122, #2448, #7411 ) ;
#7822 = CARTESIAN_POINT ( 'NONE',  ( 3.426491571325181340, -0.9799999999999436939, 2.360000000000016307 ) ) ;
#7823 = DIRECTION ( 'NONE',  ( -0.7071067811865474617, 0.7071067811865474617, 0.000000000000000000 ) ) ;
#7824 = CARTESIAN_POINT ( 'NONE',  ( -0.4424999999999982836, -0.6590000000000000302, 0.3724999999999999423 ) ) ;
#7825 = ORIENTED_EDGE ( 'NONE', *, *, #1206, .T. ) ;
#7826 = EDGE_CURVE ( 'NONE', #5805, #4636, #4680, .T. ) ;
#7827 = DIRECTION ( 'NONE',  ( 0.000000000000000000, 0.000000000000000000, 1.000000000000000000 ) ) ;
#7828 = B_SPLINE_CURVE_WITH_KNOTS ( 'NONE', 3,
 ( #3293, #7882, #14839, #11169, #12611, #2133, #5443, #670, #7812, #14762, #13604, #10188, #3150, #1980, #979, #8881, #10038, #6665, #12388, #5670, #6826, #11479, #14694, #4219, #4373, #13525, #3066, #9039, #1904, #6593, #12534, #11554, #8048, #5744, #1213, #9497, #10410, #8281, #6973, #2291, #15072, #2374, #2453, #4517, #12923, #11632, #12695, #14062, #5903, #9188, #10559, #14147 ),
 .UNSPECIFIED., .F., .F.,
 ( 4, 2, 2, 2, 2, 2, 2, 2, 2, 2, 2, 2, 2, 2, 2, 2, 2, 2, 2, 2, 2, 2, 2, 2, 2, 4 ),
 ( 0.000000000000000000, 0.002524598796828807657, 0.003786898195243190886, 0.005049197593657573681, 0.007573796390486340138, 0.008836095788900722933, 0.01009839518731510573, 0.01136069458572948852, 0.01262299398414387305, 0.01514759278097261783, 0.01640989217938699368, 0.01767219157780136607, 0.02019679037463009696, 0.02145908977304446935, 0.02272138917145883827, 0.02398368856987320719, 0.02524598796828757610, 0.02777058676511630700, 0.02903288616353066204, 0.03029518556194501361, 0.03281978435877375144, 0.03408208375718813771, 0.03534438315560252397, 0.03660668255401691024, 0.03786898195243129650, 0.04039358074926006209 ),
 .UNSPECIFIED. ) ;
#7829 = CARTESIAN_POINT ( 'NONE',  ( 0.8999999999999998002, 0.000000000000000000, -0.4850000000000000977 ) ) ;
#7830 = DIRECTION ( 'NONE',  ( 0.4999999999999998890, 0.000000000000000000, -0.8660254037844385966 ) ) ;
#7831 = EDGE_LOOP ( 'NONE', ( #13152, #1828, #5780, #13233 ) ) ;
#7832 = VERTEX_POINT ( 'NONE', #7137 ) ;
#7833 = FACE_OUTER_BOUND ( 'NONE', #13117, .T. ) ;
#7834 = ORIENTED_EDGE ( 'NONE', *, *, #88, .F. ) ;
#7835 = DIRECTION ( 'NONE',  ( 0.9999002670844989726, -0.000000000000000000, -0.01412288512831212997 ) ) ;
#7836 = EDGE_CURVE ( 'NONE', #9252, #801, #11386, .T. ) ;
#7837 = DIRECTION ( 'NONE',  ( 0.000000000000000000, 0.000000000000000000, -1.000000000000000000 ) ) ;
#7838 = EDGE_CURVE ( 'NONE', #8947, #3706, #857, .T. ) ;
#7839 = DIRECTION ( 'NONE',  ( -0.7071067811865459074, 8.659560562354951347E-17, -0.7071067811865490160 ) ) ;
#7840 = CARTESIAN_POINT ( 'NONE',  ( 3.631700695736539863, 1.967759286096487203, 0.4374246074370377046 ) ) ;
#7841 = VECTOR ( 'NONE', #7027, 39.37007874015748143 ) ;
#7842 = DIRECTION ( 'NONE',  ( 1.000000000000000000, 0.000000000000000000, 0.000000000000000000 ) ) ;
#7843 = ADVANCED_FACE ( 'NONE', ( #3607, #11861, #3688 ), #61, .T. ) ;
#7844 = ORIENTED_EDGE ( 'NONE', *, *, #11424, .F. ) ;
#7845 = ADVANCED_FACE ( 'NONE', ( #8129 ), #9454, .F. ) ;
#7846 = CARTESIAN_POINT ( 'NONE',  ( 4.215636577467320123, 1.714906460358956553, -0.7183765618090157679 ) ) ;
#7847 = ORIENTED_EDGE ( 'NONE', *, *, #10103, .T. ) ;
#7848 = ORIENTED_EDGE ( 'NONE', *, *, #3855, .F. ) ;
#7849 = EDGE_LOOP ( 'NONE', ( #11139, #4702, #13967, #12789 ) ) ;
#7850 = AXIS2_PLACEMENT_3D ( 'NONE', #13806, #8018, #3801 ) ;
#7851 = CARTESIAN_POINT ( 'NONE',  ( 3.874999999999999556, 3.567999999999999616, -1.097499999999999920 ) ) ;
#7852 = CARTESIAN_POINT ( 'NONE',  ( 6.176491571325181340, -1.679378605318048390, 1.272378605318051914 ) ) ;
#7853 = CARTESIAN_POINT ( 'NONE',  ( 0.7834577061006936516, -0.4429999999999997273, -0.3569559810110801146 ) ) ;
#7854 = DIRECTION ( 'NONE',  ( 1.000000000000000000, 0.000000000000000000, 0.000000000000000000 ) ) ;
#7855 = ORIENTED_EDGE ( 'NONE', *, *, #1226, .F. ) ;
#7856 = CARTESIAN_POINT ( 'NONE',  ( 3.193060682217703228, 2.480829671764972044, -0.3101105498922617221 ) ) ;
#7857 = CARTESIAN_POINT ( 'NONE',  ( 0.2100000000000001865, 1.239999999999999991, -0.3809527529760087239 ) ) ;
#7858 = SURFACE_STYLE_USAGE ( .BOTH. , #872 ) ;
#7859 = EDGE_CURVE ( 'NONE', #6548, #10691, #10899, .T. ) ;
#7860 = VECTOR ( 'NONE', #11900, 39.37007874015748143 ) ;
#7861 = CARTESIAN_POINT ( 'NONE',  ( 0.9372784336483218626, -0.4451370293985828508, -0.4407327033732494348 ) ) ;
#7862 = CARTESIAN_POINT ( 'NONE',  ( 4.039574151569903293, 1.760598961795517781, 0.7330370523027112117 ) ) ;
#7864 = EDGE_LOOP ( 'NONE', ( #2196, #4152, #13589, #13949 ) ) ;
#7863 = CARTESIAN_POINT ( 'NONE',  ( 3.447700738689755795, 2.048569235149967582, -0.2640414659212462767 ) ) ;
#7865 = ADVANCED_FACE ( 'NONE', ( #13068 ), #8286, .F. ) ;
#7866 = ORIENTED_EDGE ( 'NONE', *, *, #9316, .F. ) ;
#7868 = ORIENTED_EDGE ( 'NONE', *, *, #1632, .F. ) ;
#7867 = PLANE ( 'NONE',  #8711 ) ;
#7869 = VERTEX_POINT ( 'NONE', #10564 ) ;
#7870 = CARTESIAN_POINT ( 'NONE',  ( 2.774999999999999911, 3.360000000000016751, 0.9799999999999461364 ) ) ;
#7871 =( NAMED_UNIT ( * ) SI_UNIT ( $, .STERADIAN. ) SOLID_ANGLE_UNIT ( ) );
#7872 = CYLINDRICAL_SURFACE ( 'NONE', #10384, 1.350000000000000089 ) ;
#7873 = ORIENTED_EDGE ( 'NONE', *, *, #2865, .T. ) ;
#7874 = CARTESIAN_POINT ( 'NONE',  ( 6.794491571325179891, 1.679378605318035733, -1.304378605318064821 ) ) ;
#7875 = DIRECTION ( 'NONE',  ( 0.000000000000000000, 0.000000000000000000, 1.000000000000000000 ) ) ;
#7876 = DIRECTION ( 'NONE',  ( -0.000000000000000000, -0.000000000000000000, -1.000000000000000000 ) ) ;
#7877 = CARTESIAN_POINT ( 'NONE',  ( 2.187203820042824542, 0.4712135623730921985, -0.4085020630706684974 ) ) ;
#7878 = CARTESIAN_POINT ( 'NONE',  ( 0.5400755080658357077, 0.000000000000000000, -1.532626322880899838 ) ) ;
#7879 = AXIS2_PLACEMENT_3D ( 'NONE', #11024, #9733, #6145 ) ;
#7880 = ORIENTED_EDGE ( 'NONE', *, *, #11100, .F. ) ;
#7881 = CARTESIAN_POINT ( 'NONE',  ( 2.592367411162173507, 0.4049457270506671147, 0.4633846410852800468 ) ) ;
#7882 = CARTESIAN_POINT ( 'NONE',  ( 3.841336337880575158, 0.8660254037844382635, -0.5000000000000001110 ) ) ;
#7883 = CARTESIAN_POINT ( 'NONE',  ( 0.000000000000000000, 0.000000000000000000, 0.000000000000000000 ) ) ;
#7884 = ADVANCED_FACE ( 'NONE', ( #6052 ), #4983, .T. ) ;
#7885 = CARTESIAN_POINT ( 'NONE',  ( 4.083279076927434303, 0.8905985393163902142, -0.4548455386991649974 ) ) ;
#7887 = EDGE_LOOP ( 'NONE', ( #1196, #7568, #9147, #10350 ) ) ;
#7886 = DIRECTION ( 'NONE',  ( -0.000000000000000000, 0.000000000000000000, 1.000000000000000000 ) ) ;
#7888 = ORIENTED_EDGE ( 'NONE', *, *, #1639, .F. ) ;
#7889 = DIRECTION ( 'NONE',  ( 0.9992912762382414327, 0.03489602031262312859, 0.01411428356268702201 ) ) ;
#7890 = VERTEX_POINT ( 'NONE', #9350 ) ;
#7891 = DIRECTION ( 'NONE',  ( 0.000000000000000000, 0.000000000000000000, -1.000000000000000000 ) ) ;
#7892=STYLED_ITEM('',(#15178),#491);
#7893 = LINE ( 'NONE', #7822, #3720 ) ;
#7894 = CARTESIAN_POINT ( 'NONE',  ( 3.426491571325181340, -1.575000000000027489, -2.359999999999986109 ) ) ;
#7895 = VECTOR ( 'NONE', #7258, 39.37007874015748143 ) ;
#7896 = CARTESIAN_POINT ( 'NONE',  ( 0.2372115730956756152, 0.000000000000000000, -0.8852856429364902580 ) ) ;
#7897 = EDGE_LOOP ( 'NONE', ( #2442, #2928, #9938, #12480 ) ) ;
#7898 = CARTESIAN_POINT ( 'NONE',  ( 3.874999999999999556, 2.782000000000000917, -1.130000000000000560 ) ) ;
#7899 = CARTESIAN_POINT ( 'NONE',  ( 2.774999999999999911, 1.679378605318042395, -1.679378605318058604 ) ) ;
#7900 = DIRECTION ( 'NONE',  ( -0.000000000000000000, -1.000000000000000000, -0.000000000000000000 ) ) ;
#7901 = EDGE_LOOP ( 'NONE', ( #12700, #9002, #5391, #429 ) ) ;
#7902 = CARTESIAN_POINT ( 'NONE',  ( 6.826491571325181695, -1.679378605318048390, 1.679378605318054163 ) ) ;
#7903 = CARTESIAN_POINT ( 'NONE',  ( 0.000000000000000000, 0.000000000000000000, -0.2812500000000000555 ) ) ;
#7904 = CARTESIAN_POINT ( 'NONE',  ( 4.344846310392954436, 3.137999999999999901, 1.491010071662831171 ) ) ;
#7905 = ORIENTED_EDGE ( 'NONE', *, *, #680, .F. ) ;
#7906 = VECTOR ( 'NONE', #15144, 39.37007874015748143 ) ;
#7907 = DIRECTION ( 'NONE',  ( 0.000000000000000000, 0.000000000000000000, 1.000000000000000000 ) ) ;
#7908 = AXIS2_PLACEMENT_3D ( 'NONE', #13015, #1079, #11741 ) ;
#7909 = CARTESIAN_POINT ( 'NONE',  ( 0.6653223438648755428, -0.4594602905154550054, -0.4725272431374125670 ) ) ;
#7910 = CARTESIAN_POINT ( 'NONE',  ( 0.9081152184408426420, -0.4296495775394855721, -0.4649050791335925803 ) ) ;
#7911 = CARTESIAN_POINT ( 'NONE',  ( 3.652054291836392075, 1.959738311896082497, 0.4481273458576563451 ) ) ;
#7912 = ORIENTED_EDGE ( 'NONE', *, *, #8407, .T. ) ;
#7913 = CARTESIAN_POINT ( 'NONE',  ( 2.774999999999999911, 1.679378605318059048, 1.679378605318041506 ) ) ;
#7914 = CIRCLE ( 'NONE', #2034, 0.3750000000000004996 ) ;
#7915 = ADVANCED_FACE ( 'NONE', ( #8205 ), #12845, .F. ) ;
#7916 = EDGE_CURVE ( 'NONE', #13167, #14331, #9940, .T. ) ;
#7917 = ADVANCED_FACE ( 'NONE', ( #14294 ), #1516, .F. ) ;
#7918 = CARTESIAN_POINT ( 'NONE',  ( 3.946809452279758101, 1.834510758173002687, -0.7469057171082090774 ) ) ;
#7919 = ORIENTED_EDGE ( 'NONE', *, *, #9606, .F. ) ;
#7920 = ORIENTED_EDGE ( 'NONE', *, *, #11050, .F. ) ;
#7921 = DIRECTION ( 'NONE',  ( -0.000000000000000000, -1.000000000000000000, -0.000000000000000000 ) ) ;
#7922 = ORIENTED_EDGE ( 'NONE', *, *, #9186, .F. ) ;
#7923 = CARTESIAN_POINT ( 'NONE',  ( -5.764454660286586870E-18, 0.2159999999999999420, -0.7057575716915831521 ) ) ;
#7924 = EDGE_CURVE ( 'NONE', #4727, #14644, #6266, .T. ) ;
#7925 = FACE_OUTER_BOUND ( 'NONE', #1451, .T. ) ;
#7926 = FACE_OUTER_BOUND ( 'NONE', #3953, .T. ) ;
#7927 = EDGE_CURVE ( 'NONE', #13385, #9406, #4126, .T. ) ;
#7928 = CIRCLE ( 'NONE', #10627, 0.4849999999999999312 ) ;
#7929 = CARTESIAN_POINT ( 'NONE',  ( 3.875000000000000000, 1.059999999999999165, 0.000000000000000000 ) ) ;
#7930 = ORIENTED_EDGE ( 'NONE', *, *, #13561, .F. ) ;
#7931 = AXIS2_PLACEMENT_3D ( 'NONE', #13210, #12004, #14365 ) ;
#7932 = CARTESIAN_POINT ( 'NONE',  ( 3.426491571325181340, 2.426945040795776443, -0.5999481385559803925 ) ) ;
#7933 = CARTESIAN_POINT ( 'NONE',  ( 0.6842449982442360135, -0.003663068356172018755, -0.4560737988759725470 ) ) ;
#7934 =( LENGTH_UNIT ( ) NAMED_UNIT ( * ) SI_UNIT ( $, .METRE. ) );
#7935 = DIRECTION ( 'NONE',  ( -0.000000000000000000, 1.000000000000000000, 0.000000000000000000 ) ) ;
#7936 = AXIS2_PLACEMENT_3D ( 'NONE', #7042, #2277, #6961 ) ;
#7937 = CARTESIAN_POINT ( 'NONE',  ( 4.463949327178305282, 1.785655382754484766, 0.4666876780364017652 ) ) ;
#7939 = ORIENTED_EDGE ( 'NONE', *, *, #8665, .F. ) ;
#7938 = FACE_OUTER_BOUND ( 'NONE', #4909, .T. ) ;
#7940 = VECTOR ( 'NONE', #4763, 39.37007874015748143 ) ;
#7941 = ORIENTED_EDGE ( 'NONE', *, *, #6196, .F. ) ;
#7943 = ORIENTED_EDGE ( 'NONE', *, *, #3660, .F. ) ;
#7942 = FACE_OUTER_BOUND ( 'NONE', #14866, .T. ) ;
#7944 = ORIENTED_EDGE ( 'NONE', *, *, #5691, .F. ) ;
#7945 = DIRECTION ( 'NONE',  ( -1.000000000000000000, -0.000000000000000000, -0.000000000000000000 ) ) ;
#7946 = CARTESIAN_POINT ( 'NONE',  ( 0.7100000000000001865, 0.000000000000000000, 0.000000000000000000 ) ) ;
#7947 = ORIENTED_EDGE ( 'NONE', *, *, #8686, .T. ) ;
#7948 = CARTESIAN_POINT ( 'NONE',  ( 0.000000000000000000, 1.503199999999999870, -0.3439999999999999170 ) ) ;
#7949 = DIRECTION ( 'NONE',  ( -3.552713678800500929E-15, 0.000000000000000000, -1.000000000000000000 ) ) ;
#7950 = ADVANCED_FACE ( 'NONE', ( #2683, #3971, #12008, #6356, #6278 ), #503, .T. ) ;
#7951 = AXIS2_PLACEMENT_3D ( 'NONE', #3136, #13819, #11542 ) ;
#7952 = CARTESIAN_POINT ( 'NONE',  ( 0.6180000000000012150, 0.000000000000000000, 0.000000000000000000 ) ) ;
#7953 = VECTOR ( 'NONE', #14685, 39.37007874015748143 ) ;
#7954 = DIRECTION ( 'NONE',  ( 0.000000000000000000, 1.000000000000000000, 0.000000000000000000 ) ) ;
#7955 = CIRCLE ( 'NONE', #3558, 0.1249999999999999029 ) ;
#7956 = EDGE_CURVE ( 'NONE', #34, #12566, #13102, .T. ) ;
#7957 = CARTESIAN_POINT ( 'NONE',  ( 3.475290612095097043, 0.9969999999995592388, -0.4509139744054365129 ) ) ;
#7958 = CARTESIAN_POINT ( 'NONE',  ( 2.567289415621048843, 0.8512991579513186080, 0.4032946756736222604 ) ) ;
#7959 = DIRECTION ( 'NONE',  ( -1.000000000000000000, -0.000000000000000000, -0.000000000000000000 ) ) ;
#7960 = DIRECTION ( 'NONE',  ( -1.000000000000000000, 0.000000000000000000, 0.000000000000000000 ) ) ;
#7961 = CARTESIAN_POINT ( 'NONE',  ( 3.875000000000619504, 1.884022191776286714, 0.5000000000000002220 ) ) ;
#7962 = CARTESIAN_POINT ( 'NONE',  ( -0.7406097974541305806, 0.1956296296296295978, -9.087557275443343323E-17 ) ) ;
#7963 = VECTOR ( 'NONE', #15012, 39.37007874015748143 ) ;
#7964 =( BOUNDED_SURFACE ( )  B_SPLINE_SURFACE ( 3, 2, ( 
 ( #1073, #12710, #15087 ),
 ( #3699, #4619, #12942 ),
 ( #6992, #9208, #8305 ),
 ( #1304, #148, #4848 ),
 ( #8374, #13009, #8069 ),
 ( #5847, #6917, #2545 ),
 ( #11649, #6069, #9292 ),
 ( #7221, #2, #13927 ),
 ( #10507, #11877, #15008 ),
 ( #8222, #5760, #2391 ),
 ( #4536, #3463, #8140 ),
 ( #12781, #4693, #9362 ),
 ( #7074, #12859, #11735 ),
 ( #1230, #74, #4766 ) ),
 .UNSPECIFIED., .F., .F., .T. ) 
 B_SPLINE_SURFACE_WITH_KNOTS ( ( 4, 2, 2, 2, 2, 2, 4 ),
 ( 3, 3 ),
 ( 0.001551397270042531020, 0.002805300020215408929, 0.004059202770388286620, 0.004686154145474725682, 0.005313105520561163878, 0.005940056895647602940, 0.006567008270734042003 ),
 ( 0.000000000000000000, 1.000000000000000000 ),
 .UNSPECIFIED. ) 
 GEOMETRIC_REPRESENTATION_ITEM ( )  RATIONAL_B_SPLINE_SURFACE ( (
 ( 1.000000000000000000, 0.8091170061680436065, 1.000000000000000000),
 ( 1.000000000000000000, 0.8270513381946407172, 1.000000000000000000),
 ( 1.000000000000000000, 0.8430705034767305150, 1.000000000000000000),
 ( 1.000000000000000000, 0.8715016528491055237, 1.000000000000000000),
 ( 1.000000000000000000, 0.8830758126917526152, 1.000000000000000000),
 ( 1.000000000000000000, 0.8962350306361513974, 1.000000000000000000),
 ( 1.000000000000000000, 0.8997443014201252920, 1.000000000000000000),
 ( 1.000000000000000000, 0.9049100909108197532, 1.000000000000000000),
 ( 1.000000000000000000, 0.9065649576647897279, 1.000000000000000000),
 ( 1.000000000000000000, 0.9077684922225368602, 1.000000000000000000),
 ( 1.000000000000000000, 0.9073563424328562332, 1.000000000000000000),
 ( 1.000000000000000000, 0.9044691270897152746, 1.000000000000000000),
 ( 1.000000000000000000, 0.9020443801115979321, 1.000000000000000000),
 ( 1.000000000000000000, 0.8987017906623447905, 1.000000000000000000) ) ) 
 REPRESENTATION_ITEM ( '' )  SURFACE ( )  );
#7965 = CYLINDRICAL_SURFACE ( 'NONE', #4289, 0.9999999999999994449 ) ;
#7966 = CARTESIAN_POINT ( 'NONE',  ( -0.3725000000000002198, -0.6590000000000000302, -0.3725000000000000533 ) ) ;
#7967 = VERTEX_POINT ( 'NONE', #12227 ) ;
#7968 = AXIS2_PLACEMENT_3D ( 'NONE', #2676, #13134, #8568 ) ;
#7969 = AXIS2_PLACEMENT_3D ( 'NONE', #7353, #1288, #5056 ) ;
#7970 = B_SPLINE_CURVE_WITH_KNOTS ( 'NONE', 3,
 ( #3246, #11279, #3406, #8082, #14949, #4472, #12644, #7911, #7840, #2249, #6692, #6857, #12562, #2087, #6775, #11431 ),
 .UNSPECIFIED., .F., .F.,
 ( 4, 2, 2, 2, 2, 2, 2, 4 ),
 ( 0.001808351910784379481, 0.003649056555375718418, 0.005489761199967057789, 0.007330465844558396726, 0.009171170489149735663, 0.01285257977833238058, 0.01469328442292372125, 0.01653398906751506192 ),
 .UNSPECIFIED. ) ;
#7971 = CARTESIAN_POINT ( 'NONE',  ( 0.9749999999999999778, -0.4829448521957644402, -0.3685736694538739866 ) ) ;
#7972 = ORIENTED_EDGE ( 'NONE', *, *, #10034, .T. ) ;
#7973 = DIRECTION ( 'NONE',  ( -0.000000000000000000, -1.000000000000000000, -0.000000000000000000 ) ) ;
#7974 = CARTESIAN_POINT ( 'NONE',  ( 3.249780665369844002, 0.6798122612590479230, -0.3942284963568287171 ) ) ;
#7975 = ADVANCED_FACE ( 'NONE', ( #6422, #428 ), #2974, .F. ) ;
#7976 = ADVANCED_FACE ( 'NONE', ( #6201 ), #14310, .F. ) ;
#7977 = TOROIDAL_SURFACE ( 'NONE', #129, 1.580000000000000071, 0.08000000000000000167 ) ;
#7978 = CARTESIAN_POINT ( 'NONE',  ( 1.973079680968039540, -0.1265933021007059067, 0.4721316429241801949 ) ) ;
#7979 = DIRECTION ( 'NONE',  ( 1.000000000000000000, 0.000000000000000000, 0.000000000000000000 ) ) ;
#7980 = LINE ( 'NONE', #10197, #2145 ) ;
#7981 = DIRECTION ( 'NONE',  ( -1.325335837957481409E-16, 0.7071067811865369146, 0.7071067811865581199 ) ) ;
#7982 = ORIENTED_EDGE ( 'NONE', *, *, #12031, .F. ) ;
#7983 = CARTESIAN_POINT ( 'NONE',  ( 0.7856509485162610495, -0.4829999999999998739, -0.3627813902276397218 ) ) ;
#7984 = CARTESIAN_POINT ( 'NONE',  ( -0.4125000000000001998, 0.1859999999999983611, -0.4125000000000000333 ) ) ;
#7985 = ORIENTED_EDGE ( 'NONE', *, *, #12329, .T. ) ;
#7986 = DIRECTION ( 'NONE',  ( 0.000000000000000000, 0.000000000000000000, 1.000000000000000000 ) ) ;
#7987 = EDGE_LOOP ( 'NONE', ( #7041, #9628, #9585, #12019 ) ) ;
#7988 = AXIS2_PLACEMENT_3D ( 'NONE', #8501, #14512, #13144 ) ;
#7989 = CARTESIAN_POINT ( 'NONE',  ( 0.6500000000000001332, 0.000000000000000000, 0.000000000000000000 ) ) ;
#7990 = ORIENTED_EDGE ( 'NONE', *, *, #9786, .F. ) ;
#7991 = CARTESIAN_POINT ( 'NONE',  ( 0.000000000000000000, 4.529999999999999361, 0.000000000000000000 ) ) ;
#7992 = DIRECTION ( 'NONE',  ( 0.000000000000000000, 0.000000000000000000, -1.000000000000000000 ) ) ;
#7993 = CARTESIAN_POINT ( 'NONE',  ( 0.9861847369717875456, -0.4411715500842205429, -0.4414675945143460845 ) ) ;
#7994 = LINE ( 'NONE', #5472, #3627 ) ;
#7995 = EDGE_CURVE ( 'NONE', #8969, #7285, #14443, .T. ) ;
#7996 = AXIS2_PLACEMENT_3D ( 'NONE', #7474, #8559, #2953 ) ;
#7997 = DIRECTION ( 'NONE',  ( 0.000000000000000000, 0.000000000000000000, -1.000000000000000000 ) ) ;
#7998 = CARTESIAN_POINT ( 'NONE',  ( 8.850000000000001421, 0.8819999999999995621, 6.829619984160658046E-17 ) ) ;
#7999 = CARTESIAN_POINT ( 'NONE',  ( 3.688348485839861635, 1.864810863078529168, -0.7265032220550791120 ) ) ;
#8000 = ORIENTED_EDGE ( 'NONE', *, *, #13641, .F. ) ;
#8001 = AXIS2_PLACEMENT_3D ( 'NONE', #2365, #10550, #1349 ) ;
#8002 = ORIENTED_EDGE ( 'NONE', *, *, #10501, .F. ) ;
#8003 = DIRECTION ( 'NONE',  ( 1.000000000000000000, 0.000000000000000000, 0.000000000000000000 ) ) ;
#8004 = EDGE_LOOP ( 'NONE', ( #942, #2390, #7819, #11176 ) ) ;
#8005 = LINE ( 'NONE', #10372, #7025 ) ;
#8006 = DIRECTION ( 'NONE',  ( 0.000000000000000000, 0.000000000000000000, -1.000000000000000000 ) ) ;
#8007 = DIRECTION ( 'NONE',  ( -0.7070715176384835265, -0.7070715176384801959, -0.009986885842354482207 ) ) ;
#8008 = CARTESIAN_POINT ( 'NONE',  ( 0.1444275314249800213, 1.589819979576903686, -0.3809527529760087239 ) ) ;
#8009 = EDGE_LOOP ( 'NONE', ( #4243, #5636, #8688, #13471 ) ) ;
#8010 = CARTESIAN_POINT ( 'NONE',  ( 3.403212434743930537, 2.431262081689471444, -0.5824845941018170770 ) ) ;
#8011 = EDGE_CURVE ( 'NONE', #14571, #11839, #1807, .T. ) ;
#8012 = EDGE_CURVE ( 'NONE', #10024, #8675, #4815, .T. ) ;
#8013 = VECTOR ( 'NONE', #10342, 39.37007874015748143 ) ;
#8014 = CARTESIAN_POINT ( 'NONE',  ( 0.6757966763794752696, -0.06127796977734757677, -0.4909001136280312649 ) ) ;
#8015 = EDGE_CURVE ( 'NONE', #2016, #6979, #5054, .T. ) ;
#8016 = DIRECTION ( 'NONE',  ( 0.000000000000000000, 0.000000000000000000, 1.000000000000000000 ) ) ;
#8017 = CIRCLE ( 'NONE', #1401, 0.4349999999999999978 ) ;
#8018 = DIRECTION ( 'NONE',  ( -0.000000000000000000, 1.000000000000000000, -0.000000000000000000 ) ) ;
#8019 = CARTESIAN_POINT ( 'NONE',  ( 3.944129661530210385, 0.000000000000000000, 0.000000000000000000 ) ) ;
#8020 = EDGE_CURVE ( 'NONE', #1969, #3733, #8473, .T. ) ;
#8021 = AXIS2_PLACEMENT_3D ( 'NONE', #15040, #12887, #176 ) ;
#8022 = CARTESIAN_POINT ( 'NONE',  ( 4.621713608558009945, 1.748414620571773881, -0.08698231708713202726 ) ) ;
#8023 = ORIENTED_EDGE ( 'NONE', *, *, #1300, .F. ) ;
#8025 = ORIENTED_EDGE ( 'NONE', *, *, #2141, .T. ) ;
#8024 = CARTESIAN_POINT ( 'NONE',  ( 2.001999999999999780, 0.000000000000000000, 0.000000000000000000 ) ) ;
#8026 = CONICAL_SURFACE ( 'NONE', #7523, 0.2624999999999997335, 0.7853981633974479459 ) ;
#8027 = VERTEX_POINT ( 'NONE', #8574 ) ;
#8029 = ORIENTED_EDGE ( 'NONE', *, *, #14387, .F. ) ;
#8028 = DIRECTION ( 'NONE',  ( 0.000000000000000000, 0.000000000000000000, 1.000000000000000000 ) ) ;
#8030 = ORIENTED_EDGE ( 'NONE', *, *, #1694, .F. ) ;
#8031 = CARTESIAN_POINT ( 'NONE',  ( 0.000000000000000000, 1.249999999999999778, 0.000000000000000000 ) ) ;
#8032 = CARTESIAN_POINT ( 'NONE',  ( 3.234999999999999876, 1.679378605318059048, 1.679378605318041506 ) ) ;
#8033 = DIRECTION ( 'NONE',  ( 0.000000000000000000, 0.000000000000000000, -1.000000000000000000 ) ) ;
#8034 = ORIENTED_EDGE ( 'NONE', *, *, #3749, .T. ) ;
#8035 = TOROIDAL_SURFACE ( 'NONE', #5340, 0.8653656741516848605, 0.05999999999999999778 ) ;
#8036 = LINE ( 'NONE', #14984, #6244 ) ;
#8037 = DIRECTION ( 'NONE',  ( 0.7071067811865551223, 8.659560562354841646E-17, 0.7071067811865400232 ) ) ;
#8038 = EDGE_CURVE ( 'NONE', #2396, #13435, #8714, .T. ) ;
#8039 = AXIS2_PLACEMENT_3D ( 'NONE', #11249, #9038, #13682 ) ;
#8040 = AXIS2_PLACEMENT_3D ( 'NONE', #11714, #2132, #13981 ) ;
#8041 = DIRECTION ( 'NONE',  ( 0.000000000000000000, 0.000000000000000000, 1.000000000000000000 ) ) ;
#8042 = CIRCLE ( 'NONE', #7073, 1.000000000000000000 ) ;
#8043 = DIRECTION ( 'NONE',  ( -0.000000000000000000, -0.000000000000000000, -1.000000000000000000 ) ) ;
#8044 = CIRCLE ( 'NONE', #2408, 3.000000000000000444 ) ;
#8045 = DIRECTION ( 'NONE',  ( 0.000000000000000000, 0.000000000000000000, -1.000000000000000000 ) ) ;
#8046 = DIRECTION ( 'NONE',  ( -1.000000000000000000, -0.000000000000000000, -0.000000000000000000 ) ) ;
#8047 = CIRCLE ( 'NONE', #1919, 0.08500000000000004774 ) ;
#8048 = CARTESIAN_POINT ( 'NONE',  ( 3.407628221657749368, 0.9840755583697731179, 0.1784229389202373339 ) ) ;
#8049 = VECTOR ( 'NONE', #11023, 39.37007874015748854 ) ;
#8050 = CARTESIAN_POINT ( 'NONE',  ( 3.586764729049507050, 1.881086719192986534, -0.7575506356649558404 ) ) ;
#8051 = ADVANCED_FACE ( 'NONE', ( #11074 ), #6035, .F. ) ;
#8052 = CIRCLE ( 'NONE', #4618, 1.932031071636253650 ) ;
#8053 = DIRECTION ( 'NONE',  ( -1.000000000000000000, -0.000000000000000000, -0.000000000000000000 ) ) ;
#8055 = ORIENTED_EDGE ( 'NONE', *, *, #14297, .F. ) ;
#8054 = DIRECTION ( 'NONE',  ( -1.655665450705613915E-16, 0.000000000000000000, -1.000000000000000000 ) ) ;
#8056 = ORIENTED_EDGE ( 'NONE', *, *, #7330, .T. ) ;
#8057 = CIRCLE ( 'NONE', #3650, 0.2945000000000006501 ) ;
#8058 = EDGE_CURVE ( 'NONE', #4107, #5449, #9937, .T. ) ;
#8059 = CARTESIAN_POINT ( 'NONE',  ( 3.444319122601930972E-17, 1.591999999999999638, 0.2812500000000000555 ) ) ;
#8060 = AXIS2_PLACEMENT_3D ( 'NONE', #14667, #2814, #7483 ) ;
#8061 = ORIENTED_EDGE ( 'NONE', *, *, #10749, .F. ) ;
#8062 = DIRECTION ( 'NONE',  ( 1.000000000000000000, 0.000000000000000000, 0.000000000000000000 ) ) ;
#8063 = CARTESIAN_POINT ( 'NONE',  ( 3.390179639970222869, 0.6913388717410869910, -0.3921396980529558984 ) ) ;
#8064 = LINE ( 'NONE', #994, #4027 ) ;
#8065 = AXIS2_PLACEMENT_3D ( 'NONE', #2186, #8007, #10374 ) ;
#8066 = CARTESIAN_POINT ( 'NONE',  ( 0.9749999999999999778, -0.4829448521957645513, -0.3806875438604847561 ) ) ;
#8067 = AXIS2_PLACEMENT_3D ( 'NONE', #1858, #6394, #6243 ) ;
#8068 = ORIENTED_EDGE ( 'NONE', *, *, #8454, .T. ) ;
#8069 = CARTESIAN_POINT ( 'NONE',  ( 0.7142320474717208656, -0.4324499512733493423, 0.4648272691893456932 ) ) ;
#8070 = CARTESIAN_POINT ( 'NONE',  ( 2.774999999999999911, 0.9799999999999438050, -2.360000000000016307 ) ) ;
#8071 = ORIENTED_EDGE ( 'NONE', *, *, #14249, .F. ) ;
#8072 = DIRECTION ( 'NONE',  ( 0.000000000000000000, 0.000000000000000000, 1.000000000000000000 ) ) ;
#8073 = EDGE_LOOP ( 'NONE', ( #631, #12380, #12677, #7352 ) ) ;
#8074 = CARTESIAN_POINT ( 'NONE',  ( 3.875000000000000000, 3.137999999999999901, 0.5000000000000002220 ) ) ;
#8075 = EDGE_CURVE ( 'NONE', #13702, #8364, #142, .T. ) ;
#8076 = ADVANCED_FACE ( 'NONE', ( #3275 ), #13332, .F. ) ;
#8077 = CARTESIAN_POINT ( 'NONE',  ( 2.124999999999999556, -2.360000000000016751, -1.574999999999999956 ) ) ;
#8078 = ORIENTED_EDGE ( 'NONE', *, *, #4284, .F. ) ;
#8079 = DIRECTION ( 'NONE',  ( -1.000000000000000000, -0.000000000000000000, -0.000000000000000000 ) ) ;
#8080 = VECTOR ( 'NONE', #5739, 39.37007874015748143 ) ;
#8081 = DIRECTION ( 'NONE',  ( -1.365923996832131609E-16, 1.000000000000000000, 0.000000000000000000 ) ) ;
#8082 = CARTESIAN_POINT ( 'NONE',  ( 3.782641550552467535, 1.913069021635787736, 0.4919429857632933722 ) ) ;
#8083 = FACE_OUTER_BOUND ( 'NONE', #1948, .T. ) ;
#8084 = CARTESIAN_POINT ( 'NONE',  ( 3.725142412237626655, 1.827585193579217782, -0.7892246468208887755 ) ) ;
#8085 = ORIENTED_EDGE ( 'NONE', *, *, #5375, .F. ) ;
#8086 = ORIENTED_EDGE ( 'NONE', *, *, #11769, .F. ) ;
#8087 = EDGE_CURVE ( 'NONE', #1719, #5573, #12608, .T. ) ;
#8088 = CARTESIAN_POINT ( 'NONE',  ( 3.426491571325181340, 2.021150388955688548, 0.6098287289117807486 ) ) ;
#8089 = ORIENTED_EDGE ( 'NONE', *, *, #3548, .T. ) ;
#8090 = CARTESIAN_POINT ( 'NONE',  ( 0.8999999999999998002, 0.1749999999999999889, -0.2949999999999999289 ) ) ;
#8091 = EDGE_CURVE ( 'NONE', #13105, #2938, #2850, .T. ) ;
#8092 = CARTESIAN_POINT ( 'NONE',  ( 0.8663287207495570241, -0.4696786839792623236, -0.4423263022352180718 ) ) ;
#8093 = CARTESIAN_POINT ( 'NONE',  ( 0.7856509485162611606, -0.4429999999999998939, -0.3627813902276396663 ) ) ;
#8094 = FACE_OUTER_BOUND ( 'NONE', #11053, .T. ) ;
#8095 = ORIENTED_EDGE ( 'NONE', *, *, #8768, .F. ) ;
#8096 = DIRECTION ( 'NONE',  ( 0.000000000000000000, 0.000000000000000000, -1.000000000000000000 ) ) ;
#8097 = CARTESIAN_POINT ( 'NONE',  ( 0.6766392826275201555, -0.01683334090771668179, -0.4729147972022855195 ) ) ;
#8098 = DIRECTION ( 'NONE',  ( 0.000000000000000000, 1.000000000000000000, 0.000000000000000000 ) ) ;
#8099 = CARTESIAN_POINT ( 'NONE',  ( 2.124999999999999556, -1.679378605318059048, -1.679378605318041950 ) ) ;
#8100 = AXIS2_PLACEMENT_3D ( 'NONE', #7524, #841, #2156 ) ;
#8101 = CARTESIAN_POINT ( 'NONE',  ( 4.585279783993691183, 1.802421112337721398, 0.2480258495191786094 ) ) ;
#8103 = VERTEX_POINT ( 'NONE', #14749 ) ;
#8102 = DIRECTION ( 'NONE',  ( -1.000000000000000000, -0.000000000000000000, -0.000000000000000000 ) ) ;
#8104 = ORIENTED_EDGE ( 'NONE', *, *, #3931, .F. ) ;
#8106 = ORIENTED_EDGE ( 'NONE', *, *, #3918, .T. ) ;
#8105 = CARTESIAN_POINT ( 'NONE',  ( 0.6975252985509352577, 0.000000000000000000, 1.494001693158432786 ) ) ;
#8107 = ORIENTED_EDGE ( 'NONE', *, *, #7330, .F. ) ;
#8108 = CARTESIAN_POINT ( 'NONE',  ( 2.414213562373087374, 0.1427864376268978830, 0.5000000000000000000 ) ) ;
#8109 = DIRECTION ( 'NONE',  ( -0.03462124711963546903, -7.614375290267455991E-17, 0.9994005049267692398 ) ) ;
#8110 = DIRECTION ( 'NONE',  ( 0.000000000000000000, 1.000000000000000000, 0.000000000000000000 ) ) ;
#8111 = ORIENTED_EDGE ( 'NONE', *, *, #160, .T. ) ;
#8112 = DIRECTION ( 'NONE',  ( -1.365923996832131609E-16, 1.000000000000000000, 0.000000000000000000 ) ) ;
#8113 = CARTESIAN_POINT ( 'NONE',  ( 3.874999999999999556, 3.137999999999999901, -1.820000000000000284 ) ) ;
#8114 = FACE_OUTER_BOUND ( 'NONE', #11810, .T. ) ;
#8115 = AXIS2_PLACEMENT_3D ( 'NONE', #12487, #2002, #5316 ) ;
#8116 = DIRECTION ( 'NONE',  ( 0.000000000000000000, 1.000000000000000000, 4.591341165822158293E-16 ) ) ;
#8117 = CARTESIAN_POINT ( 'NONE',  ( 2.980731298636167370, 3.567999999999999616, -0.3249191361593797844 ) ) ;
#8118 = CARTESIAN_POINT ( 'NONE',  ( 0.007386697474241961034, -0.2214999999999999469, 0.5229781811763314359 ) ) ;
#8119 = FACE_OUTER_BOUND ( 'NONE', #2684, .T. ) ;
#8120 = SPHERICAL_SURFACE ( 'NONE', #14373, 1.000000000000000000 ) ;
#8121 = DIRECTION ( 'NONE',  ( 1.365923996832131609E-16, -1.000000000000000000, 0.000000000000000000 ) ) ;
#8122 = EDGE_CURVE ( 'NONE', #11673, #11895, #11144, .T. ) ;
#8123 = DIRECTION ( 'NONE',  ( -1.000000000000000000, -0.000000000000000000, -0.000000000000000000 ) ) ;
#8124 = ADVANCED_FACE ( 'NONE', ( #4352, #4277, #3203, #881 ), #7867, .T. ) ;
#8125 = VERTEX_POINT ( 'NONE', #13587 ) ;
#8126 = EDGE_CURVE ( 'NONE', #11005, #11602, #7264, .T. ) ;
#8127 = CIRCLE ( 'NONE', #12021, 0.06000000000000001860 ) ;
#8128 = CARTESIAN_POINT ( 'NONE',  ( 0.5400755080658357077, 0.000000000000000000, -1.532626322880899838 ) ) ;
#8129 = FACE_OUTER_BOUND ( 'NONE', #15053, .T. ) ;
#8130 = EDGE_LOOP ( 'NONE', ( #12701, #6685, #11517, #1862 ) ) ;
#8131 = CARTESIAN_POINT ( 'NONE',  ( 0.000000000000000000, 0.000000000000000000, 0.000000000000000000 ) ) ;
#8132 = ORIENTED_EDGE ( 'NONE', *, *, #6916, .T. ) ;
#8133 = DIRECTION ( 'NONE',  ( 0.000000000000000000, 1.000000000000000000, 0.000000000000000000 ) ) ;
#8134 = EDGE_CURVE ( 'NONE', #9926, #3188, #8868, .T. ) ;
#8135 = CARTESIAN_POINT ( 'NONE',  ( 3.314866445692595587, 0.7487158587811556520, -0.4531798524619690682 ) ) ;
#8136 = AXIS2_PLACEMENT_3D ( 'NONE', #4063, #12170, #13301 ) ;
#8137 = CARTESIAN_POINT ( 'NONE',  ( 3.426491571325181340, 0.000000000000000000, 0.000000000000000000 ) ) ;
#8138 = CARTESIAN_POINT ( 'NONE',  ( 0.9698268135359039421, -0.4829915030289423927, -0.4029731821154563520 ) ) ;
#8139 = VERTEX_POINT ( 'NONE', #3131 ) ;
#8140 = CARTESIAN_POINT ( 'NONE',  ( 0.7009701624869705272, -0.3993173672959148823, 0.4879883456728136837 ) ) ;
#8141 = CONICAL_SURFACE ( 'NONE', #14473, 1.932031071636253650, 0.2617993877991429685 ) ;
#8142 = DIRECTION ( 'NONE',  ( -1.000000000000000000, -0.000000000000000000, -0.000000000000000000 ) ) ;
#8143 = CIRCLE ( 'NONE', #12756, 0.7406097974541305806 ) ;
#8144 = CARTESIAN_POINT ( 'NONE',  ( 0.4193347797797013499, 0.1749999999999999889, -1.564978703518711711 ) ) ;
#8145 = ORIENTED_EDGE ( 'NONE', *, *, #8806, .F. ) ;
#8146 = CARTESIAN_POINT ( 'NONE',  ( 3.426491571325181340, 0.000000000000000000, 0.000000000000000000 ) ) ;
#8147 = ORIENTED_EDGE ( 'NONE', *, *, #8611, .T. ) ;
#8148 = AXIS2_PLACEMENT_3D ( 'NONE', #2435, #11531, #5882 ) ;
#8149 = CARTESIAN_POINT ( 'NONE',  ( -0.4108223460329293864, 5.750000000000000000, -4.303135664261188314E-15 ) ) ;
#8150 = VERTEX_POINT ( 'NONE', #4203 ) ;
#8151 = ADVANCED_FACE ( 'NONE', ( #13506 ), #2035, .T. ) ;
#8152 = FACE_OUTER_BOUND ( 'NONE', #6386, .T. ) ;
#8153 = CARTESIAN_POINT ( 'NONE',  ( 1.886930864188312684, -0.2403504688569103875, -0.4733484341216795399 ) ) ;
#8154 = EDGE_CURVE ( 'NONE', #10897, #3922, #802, .T. ) ;
#8155 = FACE_OUTER_BOUND ( 'NONE', #9996, .T. ) ;
#8156 = ADVANCED_FACE ( 'NONE', ( #5501 ), #2200, .F. ) ;
#8157 = CYLINDRICAL_SURFACE ( 'NONE', #9456, 0.3750000000000004996 ) ;
#8158 = CIRCLE ( 'NONE', #6437, 0.4070000000000058016 ) ;
#8159 = CARTESIAN_POINT ( 'NONE',  ( 3.692149047776956294, 1.926320256218450711, -0.7271669092250208077 ) ) ;
#8160 = ORIENTED_EDGE ( 'NONE', *, *, #6342, .T. ) ;
#8161 = ORIENTED_EDGE ( 'NONE', *, *, #3595, .F. ) ;
#8162 = AXIS2_PLACEMENT_3D ( 'NONE', #12702, #9282, #1222 ) ;
#8163 = PRODUCT_DEFINITION_CONTEXT ( 'detailed design', #6858, 'design' ) ;
#8164 = CARTESIAN_POINT ( 'NONE',  ( 0.4424999999999981726, -0.6589999999999996971, -0.3725000000000000533 ) ) ;
#8165 = VERTEX_POINT ( 'NONE', #10166 ) ;
#8166 = CARTESIAN_POINT ( 'NONE',  ( 0.3480879174158137412, 1.602949672542214321, -0.1589995474869895786 ) ) ;
#8167 = CARTESIAN_POINT ( 'NONE',  ( 0.9430132649493776498, -0.4732728608467155484, -0.4367770835854211109 ) ) ;
#8168 = FACE_OUTER_BOUND ( 'NONE', #3845, .T. ) ;
#8169 = PLANE ( 'NONE',  #7064 ) ;
#8170 = ORIENTED_EDGE ( 'NONE', *, *, #9557, .T. ) ;
#8171 = CYLINDRICAL_SURFACE ( 'NONE', #10252, 0.2499999999999999167 ) ;
#8172 = DIRECTION ( 'NONE',  ( 0.7071067811865452413, -0.7071067811865497932, 0.000000000000000000 ) ) ;
#8173 = AXIS2_PLACEMENT_3D ( 'NONE', #14585, #4117, #13431 ) ;
#8174 = DIRECTION ( 'NONE',  ( 0.000000000000000000, 1.000000000000000000, 0.000000000000000000 ) ) ;
#8175 = ADVANCED_FACE ( 'NONE', ( #7942 ), #12593, .T. ) ;
#8176 = LINE ( 'NONE', #12896, #7400 ) ;
#8177 = CARTESIAN_POINT ( 'NONE',  ( 4.671837851815657139, 1.730935268799050686, -0.1503661639408108985 ) ) ;
#8178 = VERTEX_POINT ( 'NONE', #963 ) ;
#8180 = ORIENTED_EDGE ( 'NONE', *, *, #14266, .T. ) ;
#8179 = CYLINDRICAL_SURFACE ( 'NONE', #14478, 2.499999999999999556 ) ;
#8181 = ORIENTED_EDGE ( 'NONE', *, *, #6524, .F. ) ;
#8182 = AXIS2_PLACEMENT_3D ( 'NONE', #3753, #2526, #8423 ) ;
#8184 = EDGE_LOOP ( 'NONE', ( #10665, #8029, #2056, #11820 ) ) ;
#8183 = DIRECTION ( 'NONE',  ( 0.000000000000000000, 0.7071067811865432429, 0.7071067811865516806 ) ) ;
#8185 = EDGE_LOOP ( 'NONE', ( #14882, #9509, #9768, #207 ) ) ;
#8186 = CARTESIAN_POINT ( 'NONE',  ( 2.774999999999999911, 2.400000000000010569, 0.6999999999999612088 ) ) ;
#8187 = DIRECTION ( 'NONE',  ( 1.660599669984757681E-17, -0.5794335423797530860, -0.8150194905431714654 ) ) ;
#8188 = CARTESIAN_POINT ( 'NONE',  ( 3.405153689607044232, 3.137999999999999901, 1.491010071662831171 ) ) ;
#8189 = VERTEX_POINT ( 'NONE', #5655 ) ;
#8190 = CARTESIAN_POINT ( 'NONE',  ( -0.009170202274341012275, 1.603403463250997696, -0.3809527529760086684 ) ) ;
#8191 = PLANE ( 'NONE',  #14874 ) ;
#8192 = CARTESIAN_POINT ( 'NONE',  ( 2.774999999999999911, 2.359999999999994547, -1.575000000000016831 ) ) ;
#8193 = DIRECTION ( 'NONE',  ( 0.01412288512831212997, 0.000000000000000000, -0.9999002670844990837 ) ) ;
#8194 = VECTOR ( 'NONE', #10760, 39.37007874015748143 ) ;
#8195 = EDGE_CURVE ( 'NONE', #6222, #3130, #6884, .T. ) ;
#8196 = DIRECTION ( 'NONE',  ( -1.000000000000000000, 0.000000000000000000, 0.000000000000000000 ) ) ;
#8197 = VECTOR ( 'NONE', #14407, 39.37007874015748143 ) ;
#8198 = AXIS2_PLACEMENT_3D ( 'NONE', #11394, #14690, #13597 ) ;
#8199 = DIRECTION ( 'NONE',  ( 0.000000000000000000, 0.000000000000000000, 1.000000000000000000 ) ) ;
#8200 = CARTESIAN_POINT ( 'NONE',  ( 0.000000000000000000, 1.000000000000000000, 0.000000000000000000 ) ) ;
#8201 = LINE ( 'NONE', #11857, #931 ) ;
#8202 = CARTESIAN_POINT ( 'NONE',  ( 4.684642132697897310, 1.733077758969720383, -0.04970726437145756710 ) ) ;
#8203 = ORIENTED_EDGE ( 'NONE', *, *, #14099, .T. ) ;
#8204 = CARTESIAN_POINT ( 'NONE',  ( 6.176491571325181340, -1.679378605318048390, 1.679378605318054163 ) ) ;
#8206 = VERTEX_POINT ( 'NONE', #1038 ) ;
#8205 = FACE_OUTER_BOUND ( 'NONE', #12718, .T. ) ;
#8207 = VERTEX_POINT ( 'NONE', #10023 ) ;
#8208 = CARTESIAN_POINT ( 'NONE',  ( 2.413794065081886764, 0.1423669403356975505, 0.4065001219506589325 ) ) ;
#8209 = CIRCLE ( 'NONE', #1578, 0.07500000000000002498 ) ;
#8210 = DIRECTION ( 'NONE',  ( 0.000000000000000000, 0.000000000000000000, -1.000000000000000000 ) ) ;
#8211 = EDGE_LOOP ( 'NONE', ( #6102, #10540, #9460, #14982 ) ) ;
#8212 = CARTESIAN_POINT ( 'NONE',  ( 0.000000000000000000, 1.109999999999999876, 0.000000000000000000 ) ) ;
#8213 = CIRCLE ( 'NONE', #4783, 0.07999999999999996003 ) ;
#8214 = CONICAL_SURFACE ( 'NONE', #8684, 0.2624999999999994560, 0.7853981633974446153 ) ;
#8215 = EDGE_CURVE ( 'NONE', #9027, #13119, #9559, .T. ) ;
#8216 = EDGE_CURVE ( 'NONE', #5394, #3609, #4894, .T. ) ;
#8217 = CARTESIAN_POINT ( 'NONE',  ( 3.875000000000000000, 3.137999999999999901, -0.5000000000000002220 ) ) ;
#8218 = EDGE_CURVE ( 'NONE', #7678, #5059, #5890, .T. ) ;
#8219 = CARTESIAN_POINT ( 'NONE',  ( 6.787121492585022509, 0.000000000000000000, 0.000000000000000000 ) ) ;
#8220 = ORIENTED_EDGE ( 'NONE', *, *, #10558, .T. ) ;
#8221 = AXIS2_PLACEMENT_3D ( 'NONE', #13701, #12634, #6920 ) ;
#8222 = CARTESIAN_POINT ( 'NONE',  ( 0.6552615383573069385, -0.4102766179311354566, 0.5074994761915148089 ) ) ;
#8223 = DIRECTION ( 'NONE',  ( 0.000000000000000000, -1.000000000000000000, 1.836536466328828134E-14 ) ) ;
#8224 = AXIS2_PLACEMENT_3D ( 'NONE', #5667, #8278, #8196 ) ;
#8225 = DIRECTION ( 'NONE',  ( -1.000000000000000000, -0.000000000000000000, 0.000000000000000000 ) ) ;
#8226 = CIRCLE ( 'NONE', #15047, 0.7849999999999958122 ) ;
#8227 = ORIENTED_EDGE ( 'NONE', *, *, #12495, .F. ) ;
#8228 = EDGE_CURVE ( 'NONE', #10474, #4313, #2356, .T. ) ;
#8229 = DIRECTION ( 'NONE',  ( 1.000000000000000000, 0.000000000000000000, 0.000000000000000000 ) ) ;
#8230 = ORIENTED_EDGE ( 'NONE', *, *, #11996, .F. ) ;
#8231 = DIRECTION ( 'NONE',  ( 0.000000000000000000, 0.000000000000000000, 1.000000000000000000 ) ) ;
#8232 = ORIENTED_EDGE ( 'NONE', *, *, #4020, .T. ) ;
#8233 = DIRECTION ( 'NONE',  ( -1.000000000000000000, 0.000000000000000000, 0.000000000000000000 ) ) ;
#8234 = VECTOR ( 'NONE', #5975, 39.37007874015748854 ) ;
#8235 = CARTESIAN_POINT ( 'NONE',  ( 2.414633059664288428, 0.1432059349180978269, -0.4658950132815782852 ) ) ;
#8236 = CIRCLE ( 'NONE', #1603, 0.7435009325572419225 ) ;
#8237 = CIRCLE ( 'NONE', #14805, 0.2225000000000012523 ) ;
#8238 = DIRECTION ( 'NONE',  ( -0.9999002670844990837, -1.110054405283695815E-35, -0.01412288512831213171 ) ) ;
#8239 = B_SPLINE_CURVE_WITH_KNOTS ( 'NONE', 3,
 ( #14959, #632, #5329, #14658, #11216, #14729, #713, #4259, #6939, #3648, #11826, #3567, #8166, #8248, #4875, #5870, #14186, #2257, #12656, #2183, #1099, #4641 ),
 .UNSPECIFIED., .F., .F.,
 ( 4, 2, 2, 2, 2, 2, 2, 2, 2, 2, 4 ),
 ( 2.884201056608390597E-07, 0.0006930185370336857482, 0.001385748653961710536, 0.002771208887817760546, 0.004156669121673812507, 0.005542129355529864902, 0.006927589589385916430, 0.008313049823241968825, 0.009698510057098019485, 0.01039124017402604135, 0.01108397029095406494 ),
 .UNSPECIFIED. ) ;
#8240 = DIRECTION ( 'NONE',  ( -1.000000000000000000, -0.000000000000000000, -0.000000000000000000 ) ) ;
#8241 = CONICAL_SURFACE ( 'NONE', #5779, 0.3750000000000004996, 0.7853981633974514986 ) ;
#8242 = CARTESIAN_POINT ( 'NONE',  ( 4.006803276264902181, 1.767389175965520032, -0.7395693964154066435 ) ) ;
#8243 = ORIENTED_EDGE ( 'NONE', *, *, #1520, .F. ) ;
#8244 = EDGE_LOOP ( 'NONE', ( #11487, #6329, #12769, #5909 ) ) ;
#8245 = EDGE_CURVE ( 'NONE', #11008, #15105, #1268, .T. ) ;
#8246 = CARTESIAN_POINT ( 'NONE',  ( 2.774999999999999911, -1.574999999999984190, 1.575000000000033040 ) ) ;
#8247 = VERTEX_POINT ( 'NONE', #9327 ) ;
#8248 = CARTESIAN_POINT ( 'NONE',  ( 0.3662167046612953003, 1.600826314462299838, -0.1275995668982097264 ) ) ;
#8249 = CIRCLE ( 'NONE', #3597, 0.07500000000000002498 ) ;
#8250 = CARTESIAN_POINT ( 'NONE',  ( 0.2099999999999999922, 0.7512260236060024354, -0.3809527529760087239 ) ) ;
#8251 = FILL_AREA_STYLE ('',( #5080 ) ) ;
#8252 = ADVANCED_FACE ( 'NONE', ( #11840 ), #12362, .F. ) ;
#8253 = DIRECTION ( 'NONE',  ( 8.659560562354988325E-17, 0.7071067811865430208, -0.7071067811865520136 ) ) ;
#8254 = ORIENTED_EDGE ( 'NONE', *, *, #9096, .T. ) ;
#8255 = CARTESIAN_POINT ( 'NONE',  ( 0.4425000000000002820, 0.2159999999999999420, -0.3725000000000000533 ) ) ;
#8256 = CONICAL_SURFACE ( 'NONE', #7743, 0.1899999999999996136, 0.7853981633974433940 ) ;
#8257 = DIRECTION ( 'NONE',  ( -0.7071067811865431318, 0.7071067811865520136, 0.000000000000000000 ) ) ;
#8258 = CARTESIAN_POINT ( 'NONE',  ( 5.567023771132172172, 0.000000000000000000, 0.000000000000000000 ) ) ;
#8259 = CONICAL_SURFACE ( 'NONE', #13593, 0.2625000000000000111, 0.7853981633974503884 ) ;
#8260 = PRESENTATION_STYLE_ASSIGNMENT (( #9244 ) ) ;
#8261 = CARTESIAN_POINT ( 'NONE',  ( 4.573996505429533954, 1.741627621165780626, 0.2781619901565121067 ) ) ;
#8262 = ORIENTED_EDGE ( 'NONE', *, *, #6661, .T. ) ;
#8264 = VERTEX_POINT ( 'NONE', #12978 ) ;
#8263 = CARTESIAN_POINT ( 'NONE',  ( 6.794491571325179891, -1.679378605318047946, -2.054378605318054163 ) ) ;
#8265 = ORIENTED_EDGE ( 'NONE', *, *, #1026, .T. ) ;
#8266 = CARTESIAN_POINT ( 'NONE',  ( 6.826491571325181695, 3.625725956530744935E-16, -2.960629921259841257 ) ) ;
#8267 = ORIENTED_EDGE ( 'NONE', *, *, #3639, .T. ) ;
#8268 = B_SPLINE_CURVE_WITH_KNOTS ( 'NONE', 3,
 ( #2247, #3244, #7993, #6927, #6774, #9067, #3403, #3100, #7910, #5630, #6856, #11509, #1010, #5700, #10361, #15021, #8455, #14176 ),
 .UNSPECIFIED., .F., .F.,
 ( 4, 2, 2, 2, 2, 2, 2, 2, 4 ),
 ( 0.000000000000000000, 0.0007116342341493022122, 0.001423268468298604424, 0.002134902702447906420, 0.002846536936597208849, 0.003558171170746511278, 0.004269805404895812839, 0.004981439639045115268, 0.005693073873194417697 ),
 .UNSPECIFIED. ) ;
#8269 = CYLINDRICAL_SURFACE ( 'NONE', #9219, 0.5000000000000001110 ) ;
#8270 = ADVANCED_FACE ( 'NONE', ( #11696 ), #8241, .F. ) ;
#8271 = DIRECTION ( 'NONE',  ( 1.000000000000000000, 0.000000000000000000, 0.000000000000000000 ) ) ;
#8272 = FACE_BOUND ( 'NONE', #2381, .T. ) ;
#8273 = ORIENTED_EDGE ( 'NONE', *, *, #2065, .F. ) ;
#8274 = DIRECTION ( 'NONE',  ( 0.5000000000000041078, 0.000000000000000000, 0.8660254037844363761 ) ) ;
#8275 = DIRECTION ( 'NONE',  ( -0.000000000000000000, -0.000000000000000000, -1.000000000000000000 ) ) ;
#8276 = LINE ( 'NONE', #6041, #9049 ) ;
#8277 = CARTESIAN_POINT ( 'NONE',  ( 0.000000000000000000, 4.529999999999999361, 0.000000000000000000 ) ) ;
#8278 = DIRECTION ( 'NONE',  ( -0.000000000000000000, -0.000000000000000000, -1.000000000000000000 ) ) ;
#8279 = AXIS2_PLACEMENT_3D ( 'NONE', #14876, #1943, #9144 ) ;
#8280 = CARTESIAN_POINT ( 'NONE',  ( 6.176491571325181340, 1.679378605318059492, 1.679378605318041506 ) ) ;
#8281 = CARTESIAN_POINT ( 'NONE',  ( 3.499818328484842755, 0.9437543736653750681, 0.3309102127597038367 ) ) ;
#8282 = CIRCLE ( 'NONE', #415, 0.1899999999999996136 ) ;
#8283 = CARTESIAN_POINT ( 'NONE',  ( 4.637971095798543608, 1.725702751024853931, 0.2671971766050545427 ) ) ;
#8284 = ORIENTED_EDGE ( 'NONE', *, *, #8767, .T. ) ;
#8285 = CARTESIAN_POINT ( 'NONE',  ( 3.875000000000000000, 1.112678268764263789, 0.000000000000000000 ) ) ;
#8287 = ORIENTED_EDGE ( 'NONE', *, *, #1743, .T. ) ;
#8286 = PLANE ( 'NONE',  #11889 ) ;
#8288 = ORIENTED_EDGE ( 'NONE', *, *, #2397, .F. ) ;
#8289 = AXIS2_PLACEMENT_3D ( 'NONE', #4516, #5743, #2373 ) ;
#8290 = DIRECTION ( 'NONE',  ( -1.000000000000000000, -0.000000000000000000, -0.000000000000000000 ) ) ;
#8291 = DIRECTION ( 'NONE',  ( -1.000000000000000000, -0.000000000000000000, -0.000000000000000000 ) ) ;
#8292 = CARTESIAN_POINT ( 'NONE',  ( -0.09035531712817639061, 1.629999999999999893, 0.1565000000000000280 ) ) ;
#8293 = ORIENTED_EDGE ( 'NONE', *, *, #3162, .T. ) ;
#8294 = VECTOR ( 'NONE', #14337, 39.37007874015748143 ) ;
#8295 = CARTESIAN_POINT ( 'NONE',  ( 3.874999999999999556, 3.137999999999999901, 1.097500000000000586 ) ) ;
#8296 = AXIS2_PLACEMENT_3D ( 'NONE', #12162, #8953, #2834 ) ;
#8297 = SHAPE_REPRESENTATION ( 'Cap Screw', ( #8424 ), #3278 ) ;
#8298 = DIRECTION ( 'NONE',  ( -1.000000000000000000, -0.000000000000000000, -0.000000000000000000 ) ) ;
#8299 = VECTOR ( 'NONE', #11967, 39.37007874015748143 ) ;
#8300 = CONICAL_SURFACE ( 'NONE', #10234, 0.5174999999999995159, 0.7853981633974514986 ) ;
#8301 = LINE ( 'NONE', #7149, #1664 ) ;
#8302 = AXIS2_PLACEMENT_3D ( 'NONE', #14437, #12991, #7200 ) ;
#8303 = VERTEX_POINT ( 'NONE', #1197 ) ;
#8304 = CIRCLE ( 'NONE', #1672, 0.05999999999999990757 ) ;
#8305 = CARTESIAN_POINT ( 'NONE',  ( 0.7350000851713975880, -0.4417469416942715332, 0.4439478790713853873 ) ) ;
#8306 = CARTESIAN_POINT ( 'NONE',  ( 6.826491571325181695, -1.679378605318048390, 1.304378605318053497 ) ) ;
#8307 = DIRECTION ( 'NONE',  ( -1.000000000000000000, -0.000000000000000000, -0.000000000000000000 ) ) ;
#8308 = ORIENTED_EDGE ( 'NONE', *, *, #1820, .F. ) ;
#8309 = CIRCLE ( 'NONE', #8772, 1.409999999999999920 ) ;
#8310 = AXIS2_PLACEMENT_3D ( 'NONE', #13496, #8630, #10012 ) ;
#8311 = DIRECTION ( 'NONE',  ( 0.9659258262890749736, -0.000000000000000000, 0.2588190451024959815 ) ) ;
#8312 = ORIENTED_EDGE ( 'NONE', *, *, #7673, .F. ) ;
#8313 = EDGE_CURVE ( 'NONE', #13454, #4101, #9253, .T. ) ;
#8314 = DIRECTION ( 'NONE',  ( 0.000000000000000000, 0.000000000000000000, -1.000000000000000000 ) ) ;
#8315 = ORIENTED_EDGE ( 'NONE', *, *, #11350, .F. ) ;
#8316 = CARTESIAN_POINT ( 'NONE',  ( 0.4529333289293680509, 0.000000000000000000, -1.690370196005881009 ) ) ;
#8317 = CIRCLE ( 'NONE', #5360, 0.4349999999999999978 ) ;
#8318 = CARTESIAN_POINT ( 'NONE',  ( 1.518565137009270316, -0.3790332973735661692, -0.4187650862911278526 ) ) ;
#8319 = VECTOR ( 'NONE', #13658, 39.37007874015748143 ) ;
#8320 = ADVANCED_FACE ( 'NONE', ( #10695 ), #14566, .F. ) ;
#8321 = FACE_OUTER_BOUND ( 'NONE', #14273, .T. ) ;
#8322 = PLANE ( 'NONE',  #14070 ) ;
#8323 = VERTEX_POINT ( 'NONE', #1343 ) ;
#8324 = ORIENTED_EDGE ( 'NONE', *, *, #3749, .F. ) ;
#8325 = EDGE_CURVE ( 'NONE', #11839, #8139, #10393, .T. ) ;
#8326 = ORIENTED_EDGE ( 'NONE', *, *, #14306, .F. ) ;
#8327 = TOROIDAL_SURFACE ( 'NONE', #14163, 0.3203340137431718859, 0.05999999999999999778 ) ;
#8328 = UNCERTAINTY_MEASURE_WITH_UNIT (LENGTH_MEASURE( 1.000000000000000082E-05 ), #14300, 'distance_accuracy_value', 'NONE');
#8329 = DIRECTION ( 'NONE',  ( 0.000000000000000000, 0.000000000000000000, -1.000000000000000000 ) ) ;
#8330 = ADVANCED_FACE ( 'NONE', ( #10544 ), #9481, .T. ) ;
#8331 = CARTESIAN_POINT ( 'NONE',  ( -5.764454660286586870E-18, -0.2214999999999999469, 0.000000000000000000 ) ) ;
#8332 = DIRECTION ( 'NONE',  ( 0.000000000000000000, -1.000000000000000000, 4.591341165821855765E-15 ) ) ;
#8333 = CARTESIAN_POINT ( 'NONE',  ( 3.426491571325181340, 3.360000000000016751, 0.9799999999999461364 ) ) ;
#8334 = ORIENTED_EDGE ( 'NONE', *, *, #7277, .F. ) ;
#8335 = LINE ( 'NONE', #12968, #11213 ) ;
#8336 = ADVANCED_FACE ( 'NONE', ( #4580 ), #2605, .F. ) ;
#8337 = CARTESIAN_POINT ( 'NONE',  ( 1.541692889559679314, 0.03598127022577071038, 0.4179989611391359827 ) ) ;
#8338 = LINE ( 'NONE', #2499, #11755 ) ;
#8339 = EDGE_CURVE ( 'NONE', #2140, #14656, #4657, .T. ) ;
#8340 = CARTESIAN_POINT ( 'NONE',  ( 1.814459835756289552, 0.1490781312163599881, -0.4743720362179413841 ) ) ;
#8341 = EDGE_LOOP ( 'NONE', ( #7772, #14275, #9335, #5321 ) ) ;
#8343 = ORIENTED_EDGE ( 'NONE', *, *, #2912, .F. ) ;
#8342 = DIRECTION ( 'NONE',  ( 0.000000000000000000, 0.000000000000000000, -1.000000000000000000 ) ) ;
#8344 = ORIENTED_EDGE ( 'NONE', *, *, #697, .T. ) ;
#8345 = DIRECTION ( 'NONE',  ( 0.000000000000000000, 0.000000000000000000, -1.000000000000000000 ) ) ;
#8346 = ORIENTED_EDGE ( 'NONE', *, *, #14592, .T. ) ;
#8347 = CARTESIAN_POINT ( 'NONE',  ( 3.874999999999999556, 2.782000000000002693, 1.509999999999999787 ) ) ;
#8348 = APPLICATION_PROTOCOL_DEFINITION ( 'draft international standard', 'automotive_design', 1998, #7067 ) ;
#8349 = CARTESIAN_POINT ( 'NONE',  ( 6.787121492585022509, 0.000000000000000000, 0.000000000000000000 ) ) ;
#8350 = ORIENTED_EDGE ( 'NONE', *, *, #10671, .F. ) ;
#8351 = FACE_OUTER_BOUND ( 'NONE', #89, .T. ) ;
#8352 = LINE ( 'NONE', #8489, #1435 ) ;
#8353 = EDGE_CURVE ( 'NONE', #7227, #11593, #4556, .T. ) ;
#8354 = DIRECTION ( 'NONE',  ( 0.000000000000000000, 0.000000000000000000, -1.000000000000000000 ) ) ;
#8355 = DIRECTION ( 'NONE',  ( 0.000000000000000000, -1.000000000000000000, -0.000000000000000000 ) ) ;
#8356 = DIRECTION ( 'NONE',  ( 0.000000000000000000, 0.000000000000000000, -1.000000000000000000 ) ) ;
#8357 = CARTESIAN_POINT ( 'NONE',  ( 0.09500000000000431710, -1.679378605318047946, -1.679378605318053497 ) ) ;
#8358 = EDGE_CURVE ( 'NONE', #12649, #8125, #2586, .T. ) ;
#8359 = DIRECTION ( 'NONE',  ( 1.000000000000000000, 0.000000000000000000, 0.000000000000000000 ) ) ;
#8360 = CARTESIAN_POINT ( 'NONE',  ( 4.685850439600122819, 1.733285504273739397, -0.02487941436545356572 ) ) ;
#8361 = ORIENTED_EDGE ( 'NONE', *, *, #12490, .T. ) ;
#8362 = CARTESIAN_POINT ( 'NONE',  ( 3.874999999999999556, 3.567999999999999616, 1.320000000000000062 ) ) ;
#8364 = VERTEX_POINT ( 'NONE', #7120 ) ;
#8363 = CARTESIAN_POINT ( 'NONE',  ( 2.742999999999998995, -1.679378605318059048, -1.679378605318041950 ) ) ;
#8365 = ORIENTED_EDGE ( 'NONE', *, *, #13370, .T. ) ;
#8366 = DIRECTION ( 'NONE',  ( 0.000000000000000000, 0.000000000000000000, 1.000000000000000000 ) ) ;
#8367 = CARTESIAN_POINT ( 'NONE',  ( 0.6583797813917272590, -0.06299305549640535351, -0.5137833636068753762 ) ) ;
#8368 = DIRECTION ( 'NONE',  ( 0.000000000000000000, 0.000000000000000000, -1.000000000000000000 ) ) ;
#8369 = ORIENTED_EDGE ( 'NONE', *, *, #14387, .T. ) ;
#8370 = CARTESIAN_POINT ( 'NONE',  ( -5.764454660286586870E-18, 0.04143956043956045082, 0.000000000000000000 ) ) ;
#8371 = DIRECTION ( 'NONE',  ( -1.655665450705613915E-16, 0.000000000000000000, -1.000000000000000000 ) ) ;
#8372 = VERTEX_POINT ( 'NONE', #113 ) ;
#8373 = EDGE_CURVE ( 'NONE', #5982, #13550, #8960, .T. ) ;
#8374 = CARTESIAN_POINT ( 'NONE',  ( 0.6676004498178099711, -0.4647306784022276482, 0.4667915867939526064 ) ) ;
#8375 = AXIS2_PLACEMENT_3D ( 'NONE', #14336, #2944, #5021 ) ;
#8376 = DIRECTION ( 'NONE',  ( -1.000000000000000000, -0.000000000000000000, -0.000000000000000000 ) ) ;
#8377 = DIRECTION ( 'NONE',  ( -1.000000000000000000, -0.000000000000000000, -0.000000000000000000 ) ) ;
#8378 = ORIENTED_EDGE ( 'NONE', *, *, #5776, .T. ) ;
#8379 = CARTESIAN_POINT ( 'NONE',  ( 0.06299999999999994493, 3.634751699869342187E-16, 2.967999999999998639 ) ) ;
#8380 = ORIENTED_EDGE ( 'NONE', *, *, #11424, .T. ) ;
#8381 = DIRECTION ( 'NONE',  ( 1.000000000000000000, 0.000000000000000000, 0.000000000000000000 ) ) ;
#8382 = VERTEX_POINT ( 'NONE', #8105 ) ;
#8383 = LINE ( 'NONE', #9796, #7953 ) ;
#8384 = CARTESIAN_POINT ( 'NONE',  ( 2.219979583769312814, -0.03321525116784886794, -0.4091553120912245767 ) ) ;
#8385 = DIRECTION ( 'NONE',  ( -1.000000000000000000, 0.000000000000000000, 0.000000000000000000 ) ) ;
#8386 = CARTESIAN_POINT ( 'NONE',  ( 2.124999999999999556, 0.000000000000000000, 0.000000000000000000 ) ) ;
#8387 = CIRCLE ( 'NONE', #10326, 0.2224999999999996148 ) ;
#8388 = ADVANCED_BREP_SHAPE_REPRESENTATION ( '', ( #5553, #8424 ), #3023 ) ;
#8389 = EDGE_LOOP ( 'NONE', ( #11516, #1885, #4869, #5353 ) ) ;
#8390 = ORIENTED_EDGE ( 'NONE', *, *, #849, .T. ) ;
#8391 = ORIENTED_EDGE ( 'NONE', *, *, #1028, .F. ) ;
#8392 = CARTESIAN_POINT ( 'NONE',  ( 1.000000000000000222, -0.4429999999999998939, -0.3182109165419975683 ) ) ;
#8393 = DIRECTION ( 'NONE',  ( 1.000000000000000000, 0.000000000000000000, 0.000000000000000000 ) ) ;
#8394 = LINE ( 'NONE', #12963, #10555 ) ;
#8395 = CARTESIAN_POINT ( 'NONE',  ( 2.774999999999999911, -2.360000000000000320, 1.575000000000016387 ) ) ;
#8396 = ORIENTED_EDGE ( 'NONE', *, *, #13397, .F. ) ;
#8397 = CARTESIAN_POINT ( 'NONE',  ( 3.875000000000000000, 3.170499999999999208, 0.000000000000000000 ) ) ;
#8398 = CARTESIAN_POINT ( 'NONE',  ( 3.874999999999999556, 3.137999999999999901, 1.130000000000000560 ) ) ;
#8399 = CARTESIAN_POINT ( 'NONE',  ( -0.3724999999999999423, 0.000000000000000000, -0.3724999999999999978 ) ) ;
#8400 = ADVANCED_FACE ( 'NONE', ( #2272 ), #12138, .F. ) ;
#8401 = EDGE_CURVE ( 'NONE', #15103, #3470, #9871, .T. ) ;
#8402 = EDGE_CURVE ( 'NONE', #11962, #11381, #8974, .T. ) ;
#8403 = AXIS2_PLACEMENT_3D ( 'NONE', #9555, #3805, #14199 ) ;
#8404 = ORIENTED_EDGE ( 'NONE', *, *, #14377, .T. ) ;
#8406 = ORIENTED_EDGE ( 'NONE', *, *, #2088, .T. ) ;
#8405 = CARTESIAN_POINT ( 'NONE',  ( 0.4125000000000000333, 0.000000000000000000, -0.3724999999999999978 ) ) ;
#8407 = EDGE_CURVE ( 'NONE', #8947, #11381, #5111, .T. ) ;
#8408 = ORIENTED_EDGE ( 'NONE', *, *, #14212, .F. ) ;
#8409 = CARTESIAN_POINT ( 'NONE',  ( 3.876560711617219379, 3.137999999999999901, 0.000000000000000000 ) ) ;
#8410 = ORIENTED_EDGE ( 'NONE', *, *, #7826, .T. ) ;
#8411 = CARTESIAN_POINT ( 'NONE',  ( 3.875000000000000000, 1.112678268764263789, 0.000000000000000000 ) ) ;
#8412 = FACE_OUTER_BOUND ( 'NONE', #13573, .T. ) ;
#8413 = VERTEX_POINT ( 'NONE', #262 ) ;
#8414 = CIRCLE ( 'NONE', #10120, 0.5000000000000001110 ) ;
#8415 = DIRECTION ( 'NONE',  ( -1.000000000000000000, -0.000000000000000000, -0.000000000000000000 ) ) ;
#8416 = DIRECTION ( 'NONE',  ( -1.000000000000000000, -0.000000000000000000, -0.000000000000000000 ) ) ;
#8417 = AXIS2_PLACEMENT_3D ( 'NONE', #12717, #81, #3707 ) ;
#8418 = PLANE ( 'NONE',  #6605 ) ;
#8419 = DIRECTION ( 'NONE',  ( 0.000000000000000000, 1.000000000000000000, -0.000000000000000000 ) ) ;
#8420 = DIRECTION ( 'NONE',  ( -1.000000000000000000, 0.000000000000000000, 0.000000000000000000 ) ) ;
#8421 = CARTESIAN_POINT ( 'NONE',  ( 0.7983174577546989781, -0.4429999999999999494, -0.4287183451209413132 ) ) ;
#8422 = CARTESIAN_POINT ( 'NONE',  ( 2.774999999999999911, 2.360000000000000320, -0.9800000000000009814 ) ) ;
#8423 = DIRECTION ( 'NONE',  ( 0.000000000000000000, 0.000000000000000000, 1.000000000000000000 ) ) ;
#8424 = AXIS2_PLACEMENT_3D ( 'NONE', #5062, #7358, #1521 ) ;
#8425 = ORIENTED_EDGE ( 'NONE', *, *, #3996, .F. ) ;
#8426 = DIRECTION ( 'NONE',  ( 1.000000000000000000, 0.000000000000000000, 0.000000000000000000 ) ) ;
#8428 = ORIENTED_EDGE ( 'NONE', *, *, #7916, .F. ) ;
#8427 = CARTESIAN_POINT ( 'NONE',  ( 8.475037399843312613, 0.9289129992088663856, -0.3802960819231170908 ) ) ;
#8429 = ORIENTED_EDGE ( 'NONE', *, *, #849, .F. ) ;
#8430 = ADVANCED_FACE ( 'NONE', ( #1564 ), #13196, .T. ) ;
#8431 = LINE ( 'NONE', #2460, #5090 ) ;
#8432 = SHAPE_REPRESENTATION_RELATIONSHIP ( 'NONE' , 'NONE' ,  #9930, #2160 ) ;
#8433 = DIRECTION ( 'NONE',  ( -1.000000000000000000, -1.578435611247398256E-16, 0.000000000000000000 ) ) ;
#8434 = VERTEX_POINT ( 'NONE', #6115 ) ;
#8435 = CARTESIAN_POINT ( 'NONE',  ( 0.9652705920801474271, -0.4828330467331338749, -0.4119425203458967344 ) ) ;
#8436 = ADVANCED_FACE ( 'NONE', ( #14346 ), #4964, .F. ) ;
#8437 = CIRCLE ( 'NONE', #12321, 0.06000000000000001860 ) ;
#8438 = DIRECTION ( 'NONE',  ( -0.01412288512831128343, 0.000000000000000000, 0.9999002670844990837 ) ) ;
#8439 =( BOUNDED_SURFACE ( )  B_SPLINE_SURFACE ( 3, 2, ( 
 ( #4888, #14472, #9976 ),
 ( #8828, #14408, #3007 ),
 ( #14553, #463, #5160 ),
 ( #10610, #8340, #12972 ),
 ( #13398, #8605, #4003 ),
 ( #11834, #8671, #14637 ),
 ( #7597, #11110, #6026 ),
 ( #2935, #10690, #12256 ),
 ( #13243, #5227, #7522 ),
 ( #1700, #611, #7672 ) ),
 .UNSPECIFIED., .F., .F., .F. ) 
 B_SPLINE_SURFACE_WITH_KNOTS ( ( 4, 2, 2, 2, 4 ),
 ( 3, 3 ),
 ( 3.926990816987240063, 4.123340357836602799, 4.319689898685965090, 4.516039439535327382, 4.712388980384689674 ),
 ( 0.000000000000000000, 1.000000000000000000 ),
 .UNSPECIFIED. ) 
 GEOMETRIC_REPRESENTATION_ITEM ( )  RATIONAL_B_SPLINE_SURFACE ( (
 ( 1.000000000000000000, 0.7035672008258530008, 1.000000000000000000),
 ( 1.000000000000000000, 0.7037994241814377050, 1.000000000000000000),
 ( 1.000000000000000000, 0.7040544485608896119, 1.000000000000000000),
 ( 1.000000000000000000, 0.7046000480551916079, 1.000000000000000000),
 ( 1.000000000000000000, 0.7048906332649017559, 1.000000000000000000),
 ( 1.000000000000000000, 0.7054961263469431421, 1.000000000000000000),
 ( 1.000000000000000000, 0.7058110186547629228, 1.000000000000000000),
 ( 1.000000000000000000, 0.7064529522745538470, 1.000000000000000000),
 ( 1.000000000000000000, 0.7067799747770939778, 1.000000000000000000),
 ( 1.000000000000000000, 0.7071067811865475727, 1.000000000000000000) ) ) 
 REPRESENTATION_ITEM ( '' )  SURFACE ( )  );
#8440 = DIRECTION ( 'NONE',  ( 0.000000000000000000, 0.000000000000000000, 1.000000000000000000 ) ) ;
#8441 = ORIENTED_EDGE ( 'NONE', *, *, #975, .T. ) ;
#8442 = CARTESIAN_POINT ( 'NONE',  ( 0.000000000000000000, 1.866025403784438819, 0.000000000000000000 ) ) ;
#8443 = DIRECTION ( 'NONE',  ( 0.000000000000000000, 0.000000000000000000, -1.000000000000000000 ) ) ;
#8444 = DIRECTION ( 'NONE',  ( 0.000000000000000000, 0.000000000000000000, 1.000000000000000000 ) ) ;
#8445 = DIRECTION ( 'NONE',  ( 0.000000000000000000, 0.000000000000000000, 1.000000000000000000 ) ) ;
#8446 = ORIENTED_EDGE ( 'NONE', *, *, #1182, .F. ) ;
#8447 = CIRCLE ( 'NONE', #5509, 0.06999999999999823030 ) ;
#8448 = CARTESIAN_POINT ( 'NONE',  ( 2.774999999999999911, 1.574999999999994849, -1.575000000000022160 ) ) ;
#8449 = ORIENTED_EDGE ( 'NONE', *, *, #5681, .F. ) ;
#8450 = CIRCLE ( 'NONE', #5026, 2.968000000000000860 ) ;
#8451 = CARTESIAN_POINT ( 'NONE',  ( 0.7006934119264054406, -0.03740617389313986157, 0.4858827016952782518 ) ) ;
#8452 = ORIENTED_EDGE ( 'NONE', *, *, #8339, .F. ) ;
#8453 = EDGE_CURVE ( 'NONE', #11895, #5425, #157, .T. ) ;
#8454 = EDGE_CURVE ( 'NONE', #10819, #2332, #3886, .T. ) ;
#8455 = CARTESIAN_POINT ( 'NONE',  ( 0.8044756265521625371, -0.4430000000000000049, -0.4357542965500932342 ) ) ;
#8456 = CARTESIAN_POINT ( 'NONE',  ( 1.130901178792334205, -0.4429999999999999494, 0.4240763015380700773 ) ) ;
#8457 = DIRECTION ( 'NONE',  ( -0.000000000000000000, 0.000000000000000000, -1.000000000000000000 ) ) ;
#8458 = LINE ( 'NONE', #12106, #12419 ) ;
#8459 = CIRCLE ( 'NONE', #12344, 0.1150000000000000050 ) ;
#8460 = AXIS2_PLACEMENT_3D ( 'NONE', #1909, #8814, #593 ) ;
#8461 = CARTESIAN_POINT ( 'NONE',  ( 6.176491571325181340, 1.679378605318035733, -1.679378605318065487 ) ) ;
#8462 = ORIENTED_EDGE ( 'NONE', *, *, #14666, .F. ) ;
#8463 = ORIENTED_EDGE ( 'NONE', *, *, #11480, .T. ) ;
#8464 = ORIENTED_EDGE ( 'NONE', *, *, #14977, .F. ) ;
#8465 = AXIS2_PLACEMENT_3D ( 'NONE', #6133, #4832, #11637 ) ;
#8466 = CARTESIAN_POINT ( 'NONE',  ( 8.475037399843312613, 0.9289129992088663856, -0.3802960819231170353 ) ) ;
#8467 = FACE_OUTER_BOUND ( 'NONE', #12809, .T. ) ;
#8468 = AXIS2_PLACEMENT_3D ( 'NONE', #5557, #8713, #6355 ) ;
#8469 = DIRECTION ( 'NONE',  ( 1.000000000000000000, 0.000000000000000000, 0.000000000000000000 ) ) ;
#8470 = CARTESIAN_POINT ( 'NONE',  ( 3.621991451083864444, 1.943325121683542989, -0.4314162012240914112 ) ) ;
#8471 = DIRECTION ( 'NONE',  ( 1.000000000000000000, 0.000000000000000000, 0.000000000000000000 ) ) ;
#8472 = FILL_AREA_STYLE_COLOUR ( '', #10046 ) ;
#8473 = CIRCLE ( 'NONE', #14324, 0.7849999999999992539 ) ;
#8474 = FACE_OUTER_BOUND ( 'NONE', #12176, .T. ) ;
#8475 = CARTESIAN_POINT ( 'NONE',  ( 4.419074073160574656, 1.782004799223066982, -0.5191030992588754334 ) ) ;
#8476 = ORIENTED_EDGE ( 'NONE', *, *, #9895, .F. ) ;
#8478 = ORIENTED_EDGE ( 'NONE', *, *, #5816, .F. ) ;
#8477 = LINE ( 'NONE', #1850, #12286 ) ;
#8479 = ORIENTED_EDGE ( 'NONE', *, *, #3401, .F. ) ;
#8480 = FACE_OUTER_BOUND ( 'NONE', #8809, .T. ) ;
#8481 = VERTEX_POINT ( 'NONE', #1641 ) ;
#8482 = ADVANCED_FACE ( 'NONE', ( #8694 ), #15070, .F. ) ;
#8483 = CARTESIAN_POINT ( 'NONE',  ( 8.849999999999999645, 0.9399413264884247665, 6.829619984160658046E-17 ) ) ;
#8484 = AXIS2_PLACEMENT_3D ( 'NONE', #11287, #10298, #12573 ) ;
#8485 = SHAPE_DEFINITION_REPRESENTATION ( #770, #8950 ) ;
#8486 = CARTESIAN_POINT ( 'NONE',  ( 3.602264755523620465, 1.056999999999999940, 0.4491205543005138412 ) ) ;
#8487 = VERTEX_POINT ( 'NONE', #2804 ) ;
#8488 = EDGE_CURVE ( 'NONE', #4559, #7408, #11904, .T. ) ;
#8489 = CARTESIAN_POINT ( 'NONE',  ( 0.09035531712817648775, 1.379999999999999671, -0.1564999999999998892 ) ) ;
#8490 = DIRECTION ( 'NONE',  ( 0.9396926207859108704, 0.000000000000000000, -0.3420201433256620516 ) ) ;
#8491 = AXIS2_PLACEMENT_3D ( 'NONE', #12207, #1498, #6184 ) ;
#8492 = ADVANCED_FACE ( 'NONE', ( #8480 ), #11152, .F. ) ;
#8493 = PRODUCT_DEFINITION_SHAPE ( 'NONE', 'NONE',  #15161 ) ;
#8494 = DIRECTION ( 'NONE',  ( -1.000000000000000000, -0.000000000000000000, -0.000000000000000000 ) ) ;
#8495 = CARTESIAN_POINT ( 'NONE',  ( 0.8408323664393989594, -0.4817063029767711391, -0.4215754322849089575 ) ) ;
#8496 = VECTOR ( 'NONE', #12117, 39.37007874015748854 ) ;
#8497 = CARTESIAN_POINT ( 'NONE',  ( 3.687360920630248451, 1.865009923652485524, 0.7268336272103761431 ) ) ;
#8498 = DIRECTION ( 'NONE',  ( 0.000000000000000000, 9.641816448226552334E-15, 1.000000000000000000 ) ) ;
#8499 = ORIENTED_EDGE ( 'NONE', *, *, #5714, .T. ) ;
#8500 = CARTESIAN_POINT ( 'NONE',  ( 0.6940273316166114537, -0.4844395604395604904, 0.4146485309448422751 ) ) ;
#8502 = ORIENTED_EDGE ( 'NONE', *, *, #4947, .T. ) ;
#8501 = CARTESIAN_POINT ( 'NONE',  ( 0.000000000000000000, 4.529999999999999361, 0.000000000000000000 ) ) ;
#8503 = VERTEX_POINT ( 'NONE', #12206 ) ;
#8504 = EDGE_CURVE ( 'NONE', #1907, #1198, #6401, .T. ) ;
#8505 = AXIS2_PLACEMENT_3D ( 'NONE', #10476, #2594, #4970 ) ;
#8506 = DIRECTION ( 'NONE',  ( -1.000000000000000000, 0.000000000000000000, 0.000000000000000000 ) ) ;
#8507 = CARTESIAN_POINT ( 'NONE',  ( 0.6555107925675720537, -0.04007716038812948744, -0.5098556521091194282 ) ) ;
#8508 = CARTESIAN_POINT ( 'NONE',  ( 0.6179999999999965521, 1.679378605318059492, 1.679378605318041506 ) ) ;
#8509 = ORIENTED_EDGE ( 'NONE', *, *, #3468, .T. ) ;
#8510 = EDGE_CURVE ( 'NONE', #7967, #7156, #1387, .T. ) ;
#8511 = CARTESIAN_POINT ( 'NONE',  ( 3.876560711617219379, -3.000039370078740220, 0.000000000000000000 ) ) ;
#8512 = VECTOR ( 'NONE', #6929, 39.37007874015748854 ) ;
#8513 = CARTESIAN_POINT ( 'NONE',  ( 0.6609716345676563964, 0.006273129652074246713, 0.4835254040074365989 ) ) ;
#8514 = CARTESIAN_POINT ( 'NONE',  ( 6.176491571325181340, 1.679378605318059492, 1.272378605318039257 ) ) ;
#8515 = CIRCLE ( 'NONE', #1891, 0.9499999999999992895 ) ;
#8516 = EDGE_CURVE ( 'NONE', #5884, #7375, #5038, .T. ) ;
#8517 = ORIENTED_EDGE ( 'NONE', *, *, #9240, .F. ) ;
#8518 = DIRECTION ( 'NONE',  ( -0.5000000000000101030, 0.000000000000000000, -0.8660254037844328234 ) ) ;
#8519 = CARTESIAN_POINT ( 'NONE',  ( 0.6500000000000001332, -1.679378605318047946, -1.679378605318053497 ) ) ;
#8520 = CARTESIAN_POINT ( 'NONE',  ( 2.774999999999999911, -0.6999999999999587663, 2.400000000000012790 ) ) ;
#8521 = VERTEX_POINT ( 'NONE', #3257 ) ;
#8522 = EDGE_CURVE ( 'NONE', #3074, #10691, #11360, .T. ) ;
#8523 = AXIS2_PLACEMENT_3D ( 'NONE', #11979, #4951, #12122 ) ;
#8524 = LINE ( 'NONE', #13166, #13309 ) ;
#8525 = ORIENTED_EDGE ( 'NONE', *, *, #11706, .T. ) ;
#8526 = AXIS2_PLACEMENT_3D ( 'NONE', #4588, #2042, #13677 ) ;
#8527 = CARTESIAN_POINT ( 'NONE',  ( -0.4193214606628511976, 1.577645543303436648, 0.03561943137996692599 ) ) ;
#8528 = EDGE_LOOP ( 'NONE', ( #13667, #8346 ) ) ;
#8529 = DIRECTION ( 'NONE',  ( 0.000000000000000000, 0.000000000000000000, -1.000000000000000000 ) ) ;
#8530 = VECTOR ( 'NONE', #13080, 39.37007874015748143 ) ;
#8531 = DIRECTION ( 'NONE',  ( 0.000000000000000000, 1.000000000000000000, -0.000000000000000000 ) ) ;
#8532 = EDGE_CURVE ( 'NONE', #11740, #12941, #2560, .T. ) ;
#8533 = CIRCLE ( 'NONE', #9991, 0.2944999999999998175 ) ;
#8534 = CARTESIAN_POINT ( 'NONE',  ( 0.8999999999999998002, 0.1549999999999996103, -0.4650000000000000244 ) ) ;
#8535 = AXIS2_PLACEMENT_3D ( 'NONE', #3701, #8307, #11737 ) ;
#8536 = CARTESIAN_POINT ( 'NONE',  ( 0.000000000000000000, 0.000000000000000000, 0.000000000000000000 ) ) ;
#8537 = VECTOR ( 'NONE', #11450, 39.37007874015748143 ) ;
#8538 = DIRECTION ( 'NONE',  ( 0.000000000000000000, 0.000000000000000000, -1.000000000000000000 ) ) ;
#8539 = DIMENSIONAL_EXPONENTS ( 1.000000000000000000, 0.000000000000000000, 0.000000000000000000, 0.000000000000000000, 0.000000000000000000, 0.000000000000000000, 0.000000000000000000 ) ;
#8540 = EDGE_CURVE ( 'NONE', #9564, #5730, #4327, .T. ) ;
#8541 = ADVANCED_FACE ( 'NONE', ( #4185 ), #10922, .T. ) ;
#8542 = AXIS2_PLACEMENT_3D ( 'NONE', #13223, #7431, #12089 ) ;
#8543 = VERTEX_POINT ( 'NONE', #7694 ) ;
#8544 = EDGE_LOOP ( 'NONE', ( #7888, #3425, #8068, #7427 ) ) ;
#8545 = ORIENTED_EDGE ( 'NONE', *, *, #2822, .F. ) ;
#8546 = LINE ( 'NONE', #13182, #8955 ) ;
#8547 =( GEOMETRIC_REPRESENTATION_CONTEXT ( 3 ) GLOBAL_UNCERTAINTY_ASSIGNED_CONTEXT ( ( #12881 ) ) GLOBAL_UNIT_ASSIGNED_CONTEXT ( ( #2774, #10528, #11596 ) ) REPRESENTATION_CONTEXT ( 'NONE', 'WORKASPACE' ) );
#8548 = DIRECTION ( 'NONE',  ( 0.000000000000000000, 0.000000000000000000, -1.000000000000000000 ) ) ;
#8549 = DIRECTION ( 'NONE',  ( -1.000000000000000000, -0.000000000000000000, -0.000000000000000000 ) ) ;
#8550 = DIRECTION ( 'NONE',  ( 1.000000000000000000, 0.000000000000000000, 0.000000000000000000 ) ) ;
#8551 = CARTESIAN_POINT ( 'NONE',  ( 2.633946444925666874, 0.3625193201794747466, 0.5000000000000000000 ) ) ;
#8552 = AXIS2_PLACEMENT_3D ( 'NONE', #9285, #13921, #13761 ) ;
#8553 = DIRECTION ( 'NONE',  ( 1.000000000000000000, 0.000000000000000000, 0.000000000000000000 ) ) ;
#8554 = CIRCLE ( 'NONE', #2686, 0.1250000000000000278 ) ;
#8555 = EDGE_CURVE ( 'NONE', #2763, #13066, #2114, .T. ) ;
#8556 = VERTEX_POINT ( 'NONE', #9152 ) ;
#8557 = ORIENTED_EDGE ( 'NONE', *, *, #3747, .F. ) ;
#8558 = EDGE_LOOP ( 'NONE', ( #2050, #476, #12320, #8754 ) ) ;
#8559 = DIRECTION ( 'NONE',  ( -1.000000000000000000, -0.000000000000000000, -0.000000000000000000 ) ) ;
#8560 = FACE_OUTER_BOUND ( 'NONE', #6752, .T. ) ;
#8561 = CARTESIAN_POINT ( 'NONE',  ( 4.374985573136147110, 0.9999927865700640739, 0.01697967565367332343 ) ) ;
#8562 = CARTESIAN_POINT ( 'NONE',  ( 3.874999999999999112, 2.407999999999999918, 1.319999999999999618 ) ) ;
#8563 = DIRECTION ( 'NONE',  ( 0.000000000000000000, 1.000000000000000000, 0.000000000000000000 ) ) ;
#8564 = EDGE_LOOP ( 'NONE', ( #4603, #10035, #11043, #13736, #310, #4953, #10496, #11114 ) ) ;
#8565 = LINE ( 'NONE', #4190, #3361 ) ;
#8566 = DIRECTION ( 'NONE',  ( 0.000000000000000000, 0.000000000000000000, -1.000000000000000000 ) ) ;
#8567 = DIRECTION ( 'NONE',  ( -0.3420201433256620516, 0.000000000000000000, -0.9396926207859108704 ) ) ;
#8568 = DIRECTION ( 'NONE',  ( 0.000000000000000000, 0.000000000000000000, 1.000000000000000000 ) ) ;
#8569 = CARTESIAN_POINT ( 'NONE',  ( 0.8500459336821362122, -0.4777141770823781775, -0.4313442189758466272 ) ) ;
#8570 = CARTESIAN_POINT ( 'NONE',  ( 1.861463134703978916E-17, -1.002374524060224757E-18, -0.1520000000000001905 ) ) ;
#8571 = CARTESIAN_POINT ( 'NONE',  ( 6.826491571325181695, 0.000000000000000000, 0.000000000000000000 ) ) ;
#8572 = VERTEX_POINT ( 'NONE', #7923 ) ;
#8573 = CARTESIAN_POINT ( 'NONE',  ( 0.6558215032553998958, -0.4245176963943231296, 0.5012403847680007019 ) ) ;
#8575 = ORIENTED_EDGE ( 'NONE', *, *, #5401, .F. ) ;
#8574 = CARTESIAN_POINT ( 'NONE',  ( 3.426491571325181340, -2.360000000000021636, -1.574999999999999734 ) ) ;
#8576 = VERTEX_POINT ( 'NONE', #864 ) ;
#8577 = DIRECTION ( 'NONE',  ( -0.8660254037844387076, 0.000000000000000000, -0.5000000000000001110 ) ) ;
#8578 = CARTESIAN_POINT ( 'NONE',  ( 0.6570838759023788223, -0.05534809311702808265, -0.5130260770772536727 ) ) ;
#8579 = DIRECTION ( 'NONE',  ( -0.9999002670844991947, 0.000000000000000000, 0.01412288512831583534 ) ) ;
#8580 = EDGE_LOOP ( 'NONE', ( #7584, #1812, #456, #4568, #12229 ) ) ;
#8581 = CARTESIAN_POINT ( 'NONE',  ( -5.764454660286586870E-18, 0.1759999999999999065, -0.7057575716915831521 ) ) ;
#8582 = CARTESIAN_POINT ( 'NONE',  ( 0.6558077255084613366, -0.01864179535143308669, 0.5013227096633768864 ) ) ;
#8583 = EDGE_CURVE ( 'NONE', #4442, #14332, #10074, .T. ) ;
#8584 = CYLINDRICAL_SURFACE ( 'NONE', #8542, 1.000000000000000000 ) ;
#8585 = ADVANCED_FACE ( 'NONE', ( #10005 ), #7502, .F. ) ;
#8586 = ORIENTED_EDGE ( 'NONE', *, *, #4590, .T. ) ;
#8587 = EDGE_CURVE ( 'NONE', #7304, #8264, #1789, .T. ) ;
#8588 = CARTESIAN_POINT ( 'NONE',  ( 0.000000000000000000, 1.249999999999999778, 0.000000000000000000 ) ) ;
#8589 = DIRECTION ( 'NONE',  ( 0.000000000000000000, 0.000000000000000000, -1.000000000000000000 ) ) ;
#8590 = ORIENTED_EDGE ( 'NONE', *, *, #9707, .F. ) ;
#8591 = AXIS2_PLACEMENT_3D ( 'NONE', #10282, #14942, #13775 ) ;
#8592 = DIRECTION ( 'NONE',  ( -0.3420201433256628287, 0.000000000000000000, -0.9396926207859105373 ) ) ;
#8593 = ORIENTED_EDGE ( 'NONE', *, *, #11492, .T. ) ;
#8594 = EDGE_CURVE ( 'NONE', #14846, #10200, #9952, .T. ) ;
#8595 = EDGE_CURVE ( 'NONE', #4331, #13435, #948, .T. ) ;
#8596 = FACE_BOUND ( 'NONE', #4839, .T. ) ;
#8597 = EDGE_LOOP ( 'NONE', ( #7693, #12448, #14343, #10216 ) ) ;
#8598 = B_SPLINE_CURVE_WITH_KNOTS ( 'NONE', 3,
 ( #14732, #6705, #787, #951, #9082, #4486, #8008, #14963, #7700, #5562, #7778, #6561 ),
 .UNSPECIFIED., .F., .F.,
 ( 4, 2, 2, 2, 2, 4 ),
 ( 0.000000000000000000, 0.001383149773560842519, 0.002766299547121684604, 0.004149449320682526039, 0.004841024207462948925, 0.005532599094243372678 ),
 .UNSPECIFIED. ) ;
#8599 = SURFACE_STYLE_USAGE ( .BOTH. , #14400 ) ;
#8600 = CARTESIAN_POINT ( 'NONE',  ( 2.045495128834867060, 0.3295048711651353268, -0.4105035982572215469 ) ) ;
#8601 = FACE_OUTER_BOUND ( 'NONE', #12440, .T. ) ;
#8602 = VECTOR ( 'NONE', #6316, 39.37007874015748143 ) ;
#8603 = CARTESIAN_POINT ( 'NONE',  ( 2.156999999999998696, -1.679378605318059048, -1.416878605318056872 ) ) ;
#8604 = DIRECTION ( 'NONE',  ( 0.000000000000000000, 0.000000000000000000, -1.000000000000000000 ) ) ;
#8605 = CARTESIAN_POINT ( 'NONE',  ( 1.749262710669750254, 0.1141659463772587563, -0.4752928995667935475 ) ) ;
#8606 = ORIENTED_EDGE ( 'NONE', *, *, #5691, .T. ) ;
#8607 = EDGE_LOOP ( 'NONE', ( #13632, #2731, #9117, #1061 ) ) ;
#8608 = ORIENTED_EDGE ( 'NONE', *, *, #7382, .T. ) ;
#8609 = CARTESIAN_POINT ( 'NONE',  ( 8.792093969803303821, 0.8799778768673193197, -0.04156183585338790037 ) ) ;
#8610 = CARTESIAN_POINT ( 'NONE',  ( 0.000000000000000000, 0.000000000000000000, 0.000000000000000000 ) ) ;
#8611 = EDGE_CURVE ( 'NONE', #3668, #9406, #9471, .T. ) ;
#8612 = CARTESIAN_POINT ( 'NONE',  ( 3.875000000000000000, 3.085321731235734610, 0.000000000000000000 ) ) ;
#8613 = DIRECTION ( 'NONE',  ( 0.000000000000000000, 0.000000000000000000, 1.000000000000000000 ) ) ;
#8614 = DIRECTION ( 'NONE',  ( 0.000000000000000000, -1.423315761404775650E-14, -1.000000000000000000 ) ) ;
#8615 = EDGE_CURVE ( 'NONE', #12484, #6864, #5306, .T. ) ;
#8616 = APPLICATION_CONTEXT ( 'automotive_design' ) ;
#8617 = CARTESIAN_POINT ( 'NONE',  ( 2.774999999999999911, -1.575000000000027489, -1.574999999999989297 ) ) ;
#8618 = ORIENTED_EDGE ( 'NONE', *, *, #3436, .T. ) ;
#8619 = ORIENTED_EDGE ( 'NONE', *, *, #12032, .F. ) ;
#8620 = ORIENTED_EDGE ( 'NONE', *, *, #12623, .F. ) ;
#8621 = CARTESIAN_POINT ( 'NONE',  ( 4.665325695584414469E-17, 1.603403463250997918, 0.3809527529760087239 ) ) ;
#8622 = LINE ( 'NONE', #10840, #10436 ) ;
#8623 = CARTESIAN_POINT ( 'NONE',  ( 4.006583522979322076, 0.8753738700246542770, 0.4835050455149407789 ) ) ;
#8624 = APPLICATION_PROTOCOL_DEFINITION ( 'draft international standard', 'automotive_design', 1998, #4706 ) ;
#8625 = CARTESIAN_POINT ( 'NONE',  ( 0.4124999999999997558, -0.6590000000000000302, -0.3725000000000000533 ) ) ;
#8626 = EDGE_LOOP ( 'NONE', ( #4969, #14444 ) ) ;
#8627 = DIRECTION ( 'NONE',  ( -1.000000000000000000, -0.000000000000000000, -0.000000000000000000 ) ) ;
#8628 = DIRECTION ( 'NONE',  ( 1.000000000000000000, 0.000000000000000000, 0.000000000000000000 ) ) ;
#8629 = EDGE_CURVE ( 'NONE', #1808, #3096, #13652, .T. ) ;
#8630 = DIRECTION ( 'NONE',  ( 0.000000000000000000, 0.000000000000000000, -1.000000000000000000 ) ) ;
#8631 = CIRCLE ( 'NONE', #7181, 1.000000000000000888 ) ;
#8632 = CARTESIAN_POINT ( 'NONE',  ( 0.000000000000000000, 0.04580000000000046534, 0.000000000000000000 ) ) ;
#8633 = DIRECTION ( 'NONE',  ( 0.000000000000000000, 0.000000000000000000, -1.000000000000000000 ) ) ;
#8634 = LINE ( 'NONE', #7487, #14139 ) ;
#8635 = LINE ( 'NONE', #8570, #14869 ) ;
#8636 = PLANE ( 'NONE',  #5728 ) ;
#8637 = ORIENTED_EDGE ( 'NONE', *, *, #6140, .F. ) ;
#8638 = CIRCLE ( 'NONE', #1055, 3.000000000000000444 ) ;
#8639 = LINE ( 'NONE', #11932, #11628 ) ;
#8641 = ORIENTED_EDGE ( 'NONE', *, *, #5139, .F. ) ;
#8640 = CARTESIAN_POINT ( 'NONE',  ( 0.000000000000000000, 1.224646799147353207E-16, -1.000000000000000000 ) ) ;
#8642 = ORIENTED_EDGE ( 'NONE', *, *, #2698, .F. ) ;
#8643 = CIRCLE ( 'NONE', #14487, 1.875000000000000000 ) ;
#8644 = PLANE ( 'NONE',  #13619 ) ;
#8645 = DIRECTION ( 'NONE',  ( -1.000000000000000000, -0.000000000000000000, -0.000000000000000000 ) ) ;
#8646 = VERTEX_POINT ( 'NONE', #7851 ) ;
#8647 = AXIS2_PLACEMENT_3D ( 'NONE', #11551, #3601, #5668 ) ;
#8648 = DIRECTION ( 'NONE',  ( 0.000000000000000000, 0.000000000000000000, -1.000000000000000000 ) ) ;
#8649 = CARTESIAN_POINT ( 'NONE',  ( 1.250000000000000000, 1.125000000000000000, 0.5000000000000000000 ) ) ;
#8650 = EDGE_CURVE ( 'NONE', #14113, #2273, #12499, .T. ) ;
#8651 = CARTESIAN_POINT ( 'NONE',  ( 0.7349234941866829018, -0.001280354426432115137, 0.4440226803674693912 ) ) ;
#8652 = CARTESIAN_POINT ( 'NONE',  ( -0.3725000000000002198, -0.6290000000000005587, -0.3725000000000000533 ) ) ;
#8653 = ORIENTED_EDGE ( 'NONE', *, *, #2872, .F. ) ;
#8654 = DIRECTION ( 'NONE',  ( -1.000000000000000000, 0.000000000000000000, 0.000000000000000000 ) ) ;
#8655 = DIRECTION ( 'NONE',  ( 1.000000000000000000, 0.000000000000000000, -0.000000000000000000 ) ) ;
#8656 = EDGE_LOOP ( 'NONE', ( #1155, #4942, #4354, #2468 ) ) ;
#8657 = DIRECTION ( 'NONE',  ( 0.2588190451024959260, 0.000000000000000000, -0.9659258262890748625 ) ) ;
#8658 = ORIENTED_EDGE ( 'NONE', *, *, #13093, .F. ) ;
#8659 = CARTESIAN_POINT ( 'NONE',  ( 0.7072031222531450778, -0.01850174782952182864, 0.4735570389444677675 ) ) ;
#8660 = ORIENTED_EDGE ( 'NONE', *, *, #6641, .F. ) ;
#8661 = CIRCLE ( 'NONE', #3985, 0.2625000000000000111 ) ;
#8662 = ADVANCED_FACE ( 'NONE', ( #13721 ), #8256, .F. ) ;
#8663 = PLANE ( 'NONE',  #2432 ) ;
#8664 = EDGE_CURVE ( 'NONE', #3743, #5835, #8239, .T. ) ;
#8665 = EDGE_CURVE ( 'NONE', #12434, #9682, #1861, .T. ) ;
#8666 = DIRECTION ( 'NONE',  ( -0.000000000000000000, -1.000000000000000000, -0.000000000000000000 ) ) ;
#8667 = CARTESIAN_POINT ( 'NONE',  ( 3.426491571325181340, 2.359999999999993214, -1.575000000000016831 ) ) ;
#8668 = EDGE_CURVE ( 'NONE', #11754, #4318, #9700, .T. ) ;
#8669 = AXIS2_PLACEMENT_3D ( 'NONE', #5313, #14867, #14561 ) ;
#8670 = DIRECTION ( 'NONE',  ( 0.000000000000000000, 0.000000000000000000, 1.000000000000000000 ) ) ;
#8671 = CARTESIAN_POINT ( 'NONE',  ( 1.613287804444621276, 0.05773177243533618441, -0.4772134490897831927 ) ) ;
#8672 = AXIS2_PLACEMENT_3D ( 'NONE', #14471, #610, #8538 ) ;
#8673 = VERTEX_POINT ( 'NONE', #4792 ) ;
#8674 = ORIENTED_EDGE ( 'NONE', *, *, #4284, .T. ) ;
#8675 = VERTEX_POINT ( 'NONE', #9544 ) ;
#8676 = CARTESIAN_POINT ( 'NONE',  ( 8.729039508763628774, 0.8777759665679270018, -0.1953148678277565609 ) ) ;
#8677 = LINE ( 'NONE', #3721, #2386 ) ;
#8678 = ADVANCED_FACE ( 'NONE', ( #9231 ), #1619, .F. ) ;
#8679 = CARTESIAN_POINT ( 'NONE',  ( 0.06299999999999994493, -1.679378605318048390, 1.272378605318048361 ) ) ;
#8680 = AXIS2_PLACEMENT_3D ( 'NONE', #10994, #5116, #5251 ) ;
#8681 = DIRECTION ( 'NONE',  ( 1.000000000000000000, 0.000000000000000000, 0.000000000000000000 ) ) ;
#8682 = DIRECTION ( 'NONE',  ( 0.000000000000000000, 0.000000000000000000, -1.000000000000000000 ) ) ;
#8683 = VECTOR ( 'NONE', #1162, 39.37007874015748854 ) ;
#8684 = AXIS2_PLACEMENT_3D ( 'NONE', #14660, #1869, #14428 ) ;
#8685 = CARTESIAN_POINT ( 'NONE',  ( 4.600967310741519434, 1.805377008994739185, 0.1958307185583574583 ) ) ;
#8686 = EDGE_CURVE ( 'NONE', #13039, #10392, #8005, .T. ) ;
#8687 = CIRCLE ( 'NONE', #10654, 0.2225000000000001421 ) ;
#8688 = ORIENTED_EDGE ( 'NONE', *, *, #12097, .T. ) ;
#8689 = VECTOR ( 'NONE', #8494, 39.37007874015748143 ) ;
#8690 = ORIENTED_EDGE ( 'NONE', *, *, #1286, .T. ) ;
#8691 = AXIS2_PLACEMENT_3D ( 'NONE', #3255, #14511, #11518 ) ;
#8692 = EDGE_CURVE ( 'NONE', #863, #13224, #2493, .T. ) ;
#8693 = ORIENTED_EDGE ( 'NONE', *, *, #14666, .T. ) ;
#8694 = FACE_OUTER_BOUND ( 'NONE', #4048, .T. ) ;
#8695 = DIRECTION ( 'NONE',  ( -0.000000000000000000, -1.000000000000000000, -0.000000000000000000 ) ) ;
#8696 = CARTESIAN_POINT ( 'NONE',  ( 4.370831611789263604, 0.9979212971035885671, 0.06653096183925344409 ) ) ;
#8697 = DIRECTION ( 'NONE',  ( 0.000000000000000000, 0.000000000000000000, 1.000000000000000000 ) ) ;
#8698 = ORIENTED_EDGE ( 'NONE', *, *, #6743, .T. ) ;
#8699 = LINE ( 'NONE', #6482, #5315 ) ;
#8700 = DIRECTION ( 'NONE',  ( 0.000000000000000000, 0.000000000000000000, 1.000000000000000000 ) ) ;
#8701 = AXIS2_PLACEMENT_3D ( 'NONE', #8815, #12025, #4224 ) ;
#8702 = CARTESIAN_POINT ( 'NONE',  ( 2.124999999999999556, 2.360000000000015863, 1.574999999999999956 ) ) ;
#8703 = CIRCLE ( 'NONE', #10669, 0.7057575716915831521 ) ;
#8704 = CARTESIAN_POINT ( 'NONE',  ( 8.840280274186266496, 0.9396554517976990484, 0.09865722066567160498 ) ) ;
#8705 = CARTESIAN_POINT ( 'NONE',  ( 0.9082793173477334836, -0.4296060023189146038, -0.4649570271612626371 ) ) ;
#8706 = CARTESIAN_POINT ( 'NONE',  ( 3.389020690428762084, 2.001782680153435745, 0.5706385452936350022 ) ) ;
#8708 = ORIENTED_EDGE ( 'NONE', *, *, #14322, .T. ) ;
#8707 = CARTESIAN_POINT ( 'NONE',  ( 3.405153689607044232, 3.137999999999999901, -1.491010071662831171 ) ) ;
#8709 = ADVANCED_FACE ( 'NONE', ( #12884 ), #6522, .T. ) ;
#8710 = EDGE_CURVE ( 'NONE', #6251, #6614, #13101, .T. ) ;
#8711 = AXIS2_PLACEMENT_3D ( 'NONE', #10314, #14974, #8945 ) ;
#8712 = ORIENTED_EDGE ( 'NONE', *, *, #15029, .F. ) ;
#8713 = DIRECTION ( 'NONE',  ( -2.602462600580851747E-17, -1.000000000000000000, 0.000000000000000000 ) ) ;
#8715 = ORIENTED_EDGE ( 'NONE', *, *, #6965, .F. ) ;
#8714 = LINE ( 'NONE', #13213, #1374 ) ;
#8716 = VERTEX_POINT ( 'NONE', #10526 ) ;
#8717 = DIRECTION ( 'NONE',  ( 0.000000000000000000, 0.000000000000000000, 1.000000000000000000 ) ) ;
#8718 = DIRECTION ( 'NONE',  ( -0.4999999999999998335, 0.000000000000000000, -0.8660254037844385966 ) ) ;
#8719 = ORIENTED_EDGE ( 'NONE', *, *, #12495, .T. ) ;
#8720 = AXIS2_PLACEMENT_3D ( 'NONE', #4733, #6117, #4660 ) ;
#8721 = CARTESIAN_POINT ( 'NONE',  ( 0.6975252985509352577, 0.000000000000000000, 0.000000000000000000 ) ) ;
#8722 = DIRECTION ( 'NONE',  ( 0.4999999999999979461, 0.000000000000000000, -0.8660254037844397068 ) ) ;
#8723 = DIMENSIONAL_EXPONENTS ( 1.000000000000000000, 0.000000000000000000, 0.000000000000000000, 0.000000000000000000, 0.000000000000000000, 0.000000000000000000, 0.000000000000000000 ) ;
#8724 = VECTOR ( 'NONE', #784, 39.37007874015748143 ) ;
#8725 = CARTESIAN_POINT ( 'NONE',  ( 0.6773748815706875925, -0.06659206035557797831, 0.4904325581699059966 ) ) ;
#8726 = CARTESIAN_POINT ( 'NONE',  ( 0.9747916292782434766, -0.4829471944798794381, -0.3667554846915876410 ) ) ;
#8727 = EDGE_LOOP ( 'NONE', ( #13337, #1590, #9004, #7794 ) ) ;
#8728 = LINE ( 'NONE', #1683, #9998 ) ;
#8729 = CARTESIAN_POINT ( 'NONE',  ( 3.875000000000000000, 1.059999999999999165, 0.000000000000000000 ) ) ;
#8730 = AXIS2_PLACEMENT_3D ( 'NONE', #5182, #10010, #12283 ) ;
#8731 =( CONVERSION_BASED_UNIT ( 'INCH', #7436 ) LENGTH_UNIT ( ) NAMED_UNIT ( #2954 ) );
#8732 = ORIENTED_EDGE ( 'NONE', *, *, #2469, .F. ) ;
#8733 = EDGE_CURVE ( 'NONE', #7297, #10755, #14329, .T. ) ;
#8734 = CARTESIAN_POINT ( 'NONE',  ( 4.038269563251255079, 0.8807946909871965380, -0.4737104617346509783 ) ) ;
#8735 = CARTESIAN_POINT ( 'NONE',  ( 3.874999999999999556, 3.567999999999999616, -1.320000000000000062 ) ) ;
#8736 = ORIENTED_EDGE ( 'NONE', *, *, #3950, .F. ) ;
#8737 = CARTESIAN_POINT ( 'NONE',  ( -0.3208433835780875043, 1.603403919227001762, 0.2061884643224599079 ) ) ;
#8738 = ORIENTED_EDGE ( 'NONE', *, *, #4878, .F. ) ;
#8739 = VECTOR ( 'NONE', #4267, 39.37007874015748143 ) ;
#8740 = LINE ( 'NONE', #14627, #1457 ) ;
#8741 = CONICAL_SURFACE ( 'NONE', #11922, 0.3750000000000007772, 0.7853981633974579379 ) ;
#8742 = CARTESIAN_POINT ( 'NONE',  ( 1.518565137009187049, -0.3790332973735826005, 0.4187650862912378202 ) ) ;
#8743 = CARTESIAN_POINT ( 'NONE',  ( 0.8108060929038567455, -0.4429999999999998939, -0.3024090436974092300 ) ) ;
#8744 = CARTESIAN_POINT ( 'NONE',  ( 0.09500000000000431710, -1.679378605318048390, 1.304378605318053497 ) ) ;
#8745 = DIRECTION ( 'NONE',  ( -0.000000000000000000, -1.000000000000000000, -0.000000000000000000 ) ) ;
#8746 = EDGE_CURVE ( 'NONE', #7670, #733, #3602, .T. ) ;
#8747 = CARTESIAN_POINT ( 'NONE',  ( 6.826491571325181695, 1.679378605318059492, 1.679378605318041506 ) ) ;
#8748 = AXIS2_PLACEMENT_3D ( 'NONE', #15005, #6912, #12627 ) ;
#8749 = CARTESIAN_POINT ( 'NONE',  ( 2.775039370078740131, -1.679378605318047946, -1.304378605318053053 ) ) ;
#8750 = ORIENTED_EDGE ( 'NONE', *, *, #14019, .T. ) ;
#8751 = EDGE_LOOP ( 'NONE', ( #2459, #390, #9547, #10988, #5527, #62, #13611, #880, #8844, #12730, #8921, #14601, #3156, #14413, #5976, #1340, #1702, #3573, #2580, #14465, #5008, #13523, #10268, #3248, #3940 ) ) ;
#8752 = ORIENTED_EDGE ( 'NONE', *, *, #9625, .F. ) ;
#8753 = CARTESIAN_POINT ( 'NONE',  ( 3.426491571325181340, -0.9799999999999436939, 2.360000000000016307 ) ) ;
#8754 = ORIENTED_EDGE ( 'NONE', *, *, #1210, .T. ) ;
#8755 = LINE ( 'NONE', #13407, #9155 ) ;
#8756 = AXIS2_PLACEMENT_3D ( 'NONE', #8536, #12036, #10815 ) ;
#8757 = CIRCLE ( 'NONE', #14613, 0.3750000000000004996 ) ;
#8758 = CARTESIAN_POINT ( 'NONE',  ( 6.176491571325181340, 1.679378605318059492, 1.679378605318041506 ) ) ;
#8759 = AXIS2_PLACEMENT_3D ( 'NONE', #337, #6480, #2810 ) ;
#8760 = CARTESIAN_POINT ( 'NONE',  ( 0.000000000000000000, -1.002374524060224757E-18, 0.000000000000000000 ) ) ;
#8761 = CONICAL_SURFACE ( 'NONE', #9008, 0.2219999999999999751, 0.7853981633974435050 ) ;
#8762 = CARTESIAN_POINT ( 'NONE',  ( 4.578072892439084995, 1.801135520826948166, 0.2664308559166134183 ) ) ;
#8763 = VECTOR ( 'NONE', #11335, 39.37007874015748143 ) ;
#8764 = EDGE_CURVE ( 'NONE', #12204, #4426, #11751, .T. ) ;
#8765 = VECTOR ( 'NONE', #1748, 39.37007874015748143 ) ;
#8766 = AXIS2_PLACEMENT_3D ( 'NONE', #8357, #12070, #3965 ) ;
#8767 = EDGE_CURVE ( 'NONE', #12649, #7601, #7171, .T. ) ;
#8768 = EDGE_CURVE ( 'NONE', #2309, #7417, #12805, .T. ) ;
#8769 = CONICAL_SURFACE ( 'NONE', #14872, 0.2944999999999845519, 0.7853981633974509435 ) ;
#8770 = ORIENTED_EDGE ( 'NONE', *, *, #4183, .T. ) ;
#8771 = ORIENTED_EDGE ( 'NONE', *, *, #8510, .T. ) ;
#8772 = AXIS2_PLACEMENT_3D ( 'NONE', #120, #2446, #10625 ) ;
#8773 = VECTOR ( 'NONE', #3948, 39.37007874015748143 ) ;
#8774 = ORIENTED_EDGE ( 'NONE', *, *, #4555, .F. ) ;
#8775 = CARTESIAN_POINT ( 'NONE',  ( 0.09057123220595271473, 1.599173898159329976, 0.3809527529760087239 ) ) ;
#8776 = FACE_OUTER_BOUND ( 'NONE', #3605, .T. ) ;
#8777 = FACE_OUTER_BOUND ( 'NONE', #10267, .T. ) ;
#8778 = EDGE_CURVE ( 'NONE', #9366, #3025, #8916, .T. ) ;
#8779 = CARTESIAN_POINT ( 'NONE',  ( 2.715114969688405377, 0.8546659208690539078, 0.4012693820655806598 ) ) ;
#8780 = VERTEX_POINT ( 'NONE', #7019 ) ;
#8781 = DIRECTION ( 'NONE',  ( 0.000000000000000000, 0.7071067811865441310, 0.7071067811865509034 ) ) ;
#8782 = CARTESIAN_POINT ( 'NONE',  ( 2.742999999999999883, -1.679378605318041950, 1.416878605318058870 ) ) ;
#8783 = EDGE_CURVE ( 'NONE', #12649, #12151, #12383, .T. ) ;
#8784 = CARTESIAN_POINT ( 'NONE',  ( 6.176491571325181340, 0.000000000000000000, 0.000000000000000000 ) ) ;
#8785 = CIRCLE ( 'NONE', #8065, 0.05999999999999997696 ) ;
#8786 = VECTOR ( 'NONE', #4176, 39.37007874015748143 ) ;
#8787 = CARTESIAN_POINT ( 'NONE',  ( 8.849999999999999645, 0.9399413264884969310, 0.04934655444147957593 ) ) ;
#8788 = CARTESIAN_POINT ( 'NONE',  ( 3.874999999999999556, 3.535499999999999421, 1.130000000000000560 ) ) ;
#8789 = CARTESIAN_POINT ( 'NONE',  ( 4.008086594566573346, 1.746532222454719063, 0.7851401433881748382 ) ) ;
#8791 = ORIENTED_EDGE ( 'NONE', *, *, #6387, .F. ) ;
#8790 = LINE ( 'NONE', #1511, #4762 ) ;
#8792 = ORIENTED_EDGE ( 'NONE', *, *, #13515, .T. ) ;
#8793 = DIRECTION ( 'NONE',  ( -2.602462600580851747E-17, -1.000000000000000000, 0.000000000000000000 ) ) ;
#8795 = ORIENTED_EDGE ( 'NONE', *, *, #8015, .F. ) ;
#8794 = CARTESIAN_POINT ( 'NONE',  ( 3.426491571325181340, 3.360000000000016751, 0.9799999999999461364 ) ) ;
#8796 = ORIENTED_EDGE ( 'NONE', *, *, #9557, .F. ) ;
#8797 = EDGE_CURVE ( 'NONE', #7622, #616, #10978, .T. ) ;
#8798 = AXIS2_PLACEMENT_3D ( 'NONE', #3930, #1541, #3001 ) ;
#8799 = PLANE ( 'NONE',  #10458 ) ;
#8800 = CARTESIAN_POINT ( 'NONE',  ( 8.695322983473955603, 0.9353919960747725248, 0.3771847036232494066 ) ) ;
#8801 = VERTEX_POINT ( 'NONE', #6167 ) ;
#8802 = DIRECTION ( 'NONE',  ( 1.000000000000000000, 0.000000000000000000, 0.000000000000000000 ) ) ;
#8803 = CARTESIAN_POINT ( 'NONE',  ( 6.826491571325181695, 3.649833176986402648E-16, -2.960629921259841257 ) ) ;
#8804 = EDGE_CURVE ( 'NONE', #10756, #8139, #13324, .T. ) ;
#8805 = DIRECTION ( 'NONE',  ( -1.000000000000000000, 0.000000000000000000, 0.000000000000000000 ) ) ;
#8806 = EDGE_CURVE ( 'NONE', #3024, #11151, #13252, .T. ) ;
#8807 = DIRECTION ( 'NONE',  ( 0.7071067811865474617, 8.659560562354932858E-17, 0.7071067811865474617 ) ) ;
#8808 = CARTESIAN_POINT ( 'NONE',  ( 0.3724999999999999423, -0.6290000000000003366, 0.3724999999999999423 ) ) ;
#8809 = EDGE_LOOP ( 'NONE', ( #9259, #6357, #14089, #9210 ) ) ;
#8810 = LINE ( 'NONE', #13524, #5341 ) ;
#8811 = CARTESIAN_POINT ( 'NONE',  ( 3.572912802749999006, 1.954639998949815771, 0.4011563780351515840 ) ) ;
#8812 = DIRECTION ( 'NONE',  ( 1.000000000000000000, 0.000000000000000000, 0.000000000000000000 ) ) ;
#8813 = ORIENTED_EDGE ( 'NONE', *, *, #5066, .F. ) ;
#8814 = DIRECTION ( 'NONE',  ( -1.000000000000000000, 0.000000000000000000, 0.000000000000000000 ) ) ;
#8815 = CARTESIAN_POINT ( 'NONE',  ( 3.426491571325181340, -1.679378605318059048, -1.679378605318041950 ) ) ;
#8816 = ORIENTED_EDGE ( 'NONE', *, *, #7082, .T. ) ;
#8817 = CARTESIAN_POINT ( 'NONE',  ( 0.000000000000000000, 5.750000000000000000, 0.000000000000000000 ) ) ;
#8818 = ORIENTED_EDGE ( 'NONE', *, *, #582, .T. ) ;
#8819 = AXIS2_PLACEMENT_3D ( 'NONE', #1259, #5946, #3422 ) ;
#8820 = LENGTH_MEASURE_WITH_UNIT ( LENGTH_MEASURE( 0.02539999999999999897 ), #1916 );
#8821 = DIRECTION ( 'NONE',  ( 0.000000000000000000, 0.000000000000000000, -1.000000000000000000 ) ) ;
#8822 = ADVANCED_FACE ( 'NONE', ( #248 ), #3943, .F. ) ;
#8823 = PRESENTATION_STYLE_ASSIGNMENT (( #13188 ) ) ;
#8824 = LINE ( 'NONE', #13238, #6547 ) ;
#8825 = FACE_OUTER_BOUND ( 'NONE', #10491, .T. ) ;
#8826 = ORIENTED_EDGE ( 'NONE', *, *, #15122, .T. ) ;
#8827 = FACE_OUTER_BOUND ( 'NONE', #7897, .T. ) ;
#8828 = CARTESIAN_POINT ( 'NONE',  ( 2.033926451083618581, 0.2322360065624563819, -0.4712722252671806555 ) ) ;
#8829 =( BOUNDED_SURFACE ( )  B_SPLINE_SURFACE ( 3, 2, ( 
 ( #7381, #6226, #14469 ),
 ( #10890, #3998, #5156 ),
 ( #12252, #1763, #13391 ),
 ( #9816, #12327, #14707 ),
 ( #7518, #1842, #7445 ),
 ( #6527, #4076, #2852 ),
 ( #5084, #12185, #6451 ),
 ( #6379, #9746, #13465 ),
 ( #5224, #9888, #14546 ),
 ( #8743, #4161, #11106 ) ),
 .UNSPECIFIED., .F., .F., .F. ) 
 B_SPLINE_SURFACE_WITH_KNOTS ( ( 4, 2, 2, 2, 4 ),
 ( 3, 3 ),
 ( -1.734723475976807094E-18, 0.0004185101295155288113, 0.0008370202590310593573, 0.001255530388546589795, 0.001674040518062120449 ),
 ( 0.000000000000000000, 1.000000000000000000 ),
 .UNSPECIFIED. ) 
 GEOMETRIC_REPRESENTATION_ITEM ( )  RATIONAL_B_SPLINE_SURFACE ( (
 ( 1.000000000000000000, 0.7071067811865455743, 1.000000000000000000),
 ( 1.000000000000000000, 0.6772247906454890165, 1.000000000000000000),
 ( 1.000000000000000000, 0.6514134713743581218, 1.000000000000000000),
 ( 1.000000000000000000, 0.6151943024887206457, 1.000000000000000000),
 ( 1.000000000000000000, 0.6049727253982803976, 1.000000000000000000),
 ( 1.000000000000000000, 0.6047532838980109737, 1.000000000000000000),
 ( 1.000000000000000000, 0.6149432554843776710, 1.000000000000000000),
 ( 1.000000000000000000, 0.6512885360441196259, 1.000000000000000000),
 ( 1.000000000000000000, 0.6772121499288246138, 1.000000000000000000),
 ( 1.000000000000000000, 0.7071067811865454633, 1.000000000000000000) ) ) 
 REPRESENTATION_ITEM ( '' )  SURFACE ( )  );
#8830 = DIRECTION ( 'NONE',  ( -1.000000000000000000, -0.000000000000000000, -0.000000000000000000 ) ) ;
#8831 = EDGE_LOOP ( 'NONE', ( #6698, #7240 ) ) ;
#8832 = ORIENTED_EDGE ( 'NONE', *, *, #5473, .F. ) ;
#8833 = ORIENTED_EDGE ( 'NONE', *, *, #14542, .T. ) ;
#8834 = FACE_OUTER_BOUND ( 'NONE', #14538, .T. ) ;
#8835 = VERTEX_POINT ( 'NONE', #4949 ) ;
#8836 = CARTESIAN_POINT ( 'NONE',  ( 2.774999999999999911, 1.575000000000016165, 2.359999999999999876 ) ) ;
#8837 = VECTOR ( 'NONE', #10351, 39.37007874015748143 ) ;
#8838 = DIRECTION ( 'NONE',  ( 0.000000000000000000, 0.000000000000000000, -1.000000000000000000 ) ) ;
#8839 = CARTESIAN_POINT ( 'NONE',  ( 4.111670118313984545, 1.798037458796266641, 0.7123029909491147560 ) ) ;
#8840 = EDGE_CURVE ( 'NONE', #3272, #8487, #15081, .T. ) ;
#8841 = ORIENTED_EDGE ( 'NONE', *, *, #4842, .T. ) ;
#8842 = AXIS2_PLACEMENT_3D ( 'NONE', #3570, #7104, #6018 ) ;
#8843 = CARTESIAN_POINT ( 'NONE',  ( 4.217923025938767445, 1.784679989287541346, -0.6680530993927611405 ) ) ;
#8844 = ORIENTED_EDGE ( 'NONE', *, *, #13612, .T. ) ;
#8845 = ORIENTED_EDGE ( 'NONE', *, *, #1412, .T. ) ;
#8846 = ORIENTED_EDGE ( 'NONE', *, *, #7205, .T. ) ;
#8847 = CARTESIAN_POINT ( 'NONE',  ( 3.875000000000000000, 1.885381157978844868, -0.5000000000000002220 ) ) ;
#8848 = CARTESIAN_POINT ( 'NONE',  ( 2.124999999999999556, 0.000000000000000000, 0.000000000000000000 ) ) ;
#8849 = CARTESIAN_POINT ( 'NONE',  ( 3.874999999999999556, 2.750000000000000000, 1.320000000000000062 ) ) ;
#8850 = ITEM_DEFINED_TRANSFORMATION ( 'NONE', 'NONE', #11089,  #8424 ) ;
#8851 = DIRECTION ( 'NONE',  ( 0.000000000000000000, 1.000000000000000000, 0.000000000000000000 ) ) ;
#8852 = VERTEX_POINT ( 'NONE', #9759 ) ;
#8853 = DIRECTION ( 'NONE',  ( -0.3420201433256623846, 0.000000000000000000, -0.9396926207859106484 ) ) ;
#8854 = DIRECTION ( 'NONE',  ( 1.000000000000000000, 0.000000000000000000, 0.000000000000000000 ) ) ;
#8855 = ADVANCED_FACE ( 'NONE', ( #3791 ), #6391, .F. ) ;
#8856 = EDGE_CURVE ( 'NONE', #14935, #2188, #9715, .T. ) ;
#8857 = DIRECTION ( 'NONE',  ( 0.000000000000000000, 0.000000000000000000, -1.000000000000000000 ) ) ;
#8858 = EDGE_CURVE ( 'NONE', #11912, #14728, #5166, .T. ) ;
#8859 = PRODUCT ( 'Handle', 'Handle', '', ( #4967 ) ) ;
#8860 = CARTESIAN_POINT ( 'NONE',  ( 4.344846310392954436, 3.137999999999999901, 1.491010071662831393 ) ) ;
#8861 = LINE ( 'NONE', #13500, #12037 ) ;
#8862 = ADVANCED_FACE ( 'NONE', ( #11898 ), #14479, .F. ) ;
#8863 = CARTESIAN_POINT ( 'NONE',  ( 4.336513449261514275, 1.728610328001806806, 0.5926924422214261412 ) ) ;
#8865 = ORIENTED_EDGE ( 'NONE', *, *, #7836, .T. ) ;
#8864 = FACE_OUTER_BOUND ( 'NONE', #3226, .T. ) ;
#8866 = CIRCLE ( 'NONE', #12759, 0.2944999999999998175 ) ;
#8867 = ORIENTED_EDGE ( 'NONE', *, *, #14572, .F. ) ;
#8869 = ORIENTED_EDGE ( 'NONE', *, *, #6487, .F. ) ;
#8868 = LINE ( 'NONE', #11463, #1853 ) ;
#8870 = ORIENTED_EDGE ( 'NONE', *, *, #5326, .T. ) ;
#8871 = DIRECTION ( 'NONE',  ( 0.7071067811865467956, 0.000000000000000000, -0.7071067811865482389 ) ) ;
#8872 = CARTESIAN_POINT ( 'NONE',  ( 3.875000000000000000, 3.567999999999999616, 0.5175000000000000711 ) ) ;
#8873 = VERTEX_POINT ( 'NONE', #1483 ) ;
#8874 = CARTESIAN_POINT ( 'NONE',  ( 5.296717816638158993, 3.110143505634317407, 0.3651816168881241720 ) ) ;
#8875 = FACE_OUTER_BOUND ( 'NONE', #5311, .T. ) ;
#8876 = CARTESIAN_POINT ( 'NONE',  ( 2.320261876820363334, 0.5185714323014329885, -0.4672279395929326840 ) ) ;
#8877 = CARTESIAN_POINT ( 'NONE',  ( 2.124999999999999556, -2.359999999999984333, 1.575000000000016387 ) ) ;
#8878 = VERTEX_POINT ( 'NONE', #10826 ) ;
#8879 = CARTESIAN_POINT ( 'NONE',  ( 2.814370078740158210, 0.000000000000000000, 0.000000000000000000 ) ) ;
#8880 = VECTOR ( 'NONE', #7830, 39.37007874015748854 ) ;
#8881 = CARTESIAN_POINT ( 'NONE',  ( 3.478912079112919109, 0.9522592603935663425, -0.3055730292830077799 ) ) ;
#8882 = CARTESIAN_POINT ( 'NONE',  ( 4.203702763460904102, 1.716034727807107529, -0.7239732600819549502 ) ) ;
#8883 = ADVANCED_FACE ( 'NONE', ( #8467 ), #1870, .T. ) ;
#8884 = AXIS2_PLACEMENT_3D ( 'NONE', #5219, #14537, #10744 ) ;
#8885 = DIRECTION ( 'NONE',  ( 0.000000000000000000, 1.000000000000000000, -0.000000000000000000 ) ) ;
#8886 = CARTESIAN_POINT ( 'NONE',  ( 0.8999999999999998002, 0.01999999999999975409, -0.2949999999999999289 ) ) ;
#8887 = VERTEX_POINT ( 'NONE', #7530 ) ;
#8888 = EDGE_CURVE ( 'NONE', #1001, #8887, #3871, .T. ) ;
#8889 = CARTESIAN_POINT ( 'NONE',  ( 0.9684363542373335410, -0.4829999999999998184, -0.3436319188865934460 ) ) ;
#8890 = ORIENTED_EDGE ( 'NONE', *, *, #14840, .T. ) ;
#8891 =( NAMED_UNIT ( * ) SI_UNIT ( $, .STERADIAN. ) SOLID_ANGLE_UNIT ( ) );
#8892 = CARTESIAN_POINT ( 'NONE',  ( 2.592367411162173063, 0.4049457270506676143, -0.4633846410852801023 ) ) ;
#8893 = AXIS2_PLACEMENT_3D ( 'NONE', #13942, #7842, #2007 ) ;
#8894 = CARTESIAN_POINT ( 'NONE',  ( 3.874999999999999556, 3.105999999999998984, 1.320000000000000062 ) ) ;
#8895 = DIRECTION ( 'NONE',  ( 0.000000000000000000, 0.000000000000000000, 1.000000000000000000 ) ) ;
#8896 = CYLINDRICAL_SURFACE ( 'NONE', #3303, 1.000000000000000222 ) ;
#8897 = CARTESIAN_POINT ( 'NONE',  ( 2.124999999999999556, 0.000000000000000000, 0.000000000000000000 ) ) ;
#8898 = EDGE_LOOP ( 'NONE', ( #7613, #11748, #2951, #3644 ) ) ;
#8899 = DIRECTION ( 'NONE',  ( 0.000000000000000000, 1.000000000000000000, 0.000000000000000000 ) ) ;
#8900 = DIRECTION ( 'NONE',  ( 0.000000000000000000, 0.000000000000000000, 1.000000000000000000 ) ) ;
#8901 = APPLICATION_CONTEXT ( 'automotive_design' ) ;
#8902 = VECTOR ( 'NONE', #9785, 39.37007874015748854 ) ;
#8903 = DIRECTION ( 'NONE',  ( 0.000000000000000000, -2.708891287835076765E-14, -1.000000000000000000 ) ) ;
#8904 = ORIENTED_EDGE ( 'NONE', *, *, #7106, .F. ) ;
#8905 = ORIENTED_EDGE ( 'NONE', *, *, #3480, .T. ) ;
#8906 = EDGE_CURVE ( 'NONE', #9631, #8918, #8677, .T. ) ;
#8907 = DIRECTION ( 'NONE',  ( -0.000000000000000000, -1.000000000000000000, -0.000000000000000000 ) ) ;
#8908 = ORIENTED_EDGE ( 'NONE', *, *, #3630, .F. ) ;
#8909 = LINE ( 'NONE', #4400, #8912 ) ;
#8910 = CARTESIAN_POINT ( 'NONE',  ( 0.7058998964907862161, -0.3830000000000000071, -0.4900296624789436950 ) ) ;
#8911 = DIRECTION ( 'NONE',  ( -1.000000000000000000, 0.000000000000000000, 0.000000000000000000 ) ) ;
#8912 = VECTOR ( 'NONE', #4174, 39.37007874015748143 ) ;
#8913 = CARTESIAN_POINT ( 'NONE',  ( 4.602321716688412501, 1.805624376861197700, -0.1954697140787868825 ) ) ;
#8914 = AXIS2_PLACEMENT_3D ( 'NONE', #14328, #7596, #8604 ) ;
#8915 = ORIENTED_EDGE ( 'NONE', *, *, #13004, .F. ) ;
#8916 =( BOUNDED_CURVE ( )  B_SPLINE_CURVE ( 3, ( #13870, #14109, #12732, #3486 ),
 .UNSPECIFIED., .F., .T. ) 
 B_SPLINE_CURVE_WITH_KNOTS ( ( 4, 4 ),
 ( 4.747295565424568764, 5.497787143782132624 ),
 .UNSPECIFIED. ) 
 CURVE ( )  GEOMETRIC_REPRESENTATION_ITEM ( )  RATIONAL_B_SPLINE_CURVE ( ( 1.000000000000000000, 0.9536117119880160864, 0.9536117119880160864, 1.000000000000000000 ) ) 
 REPRESENTATION_ITEM ( '' )  );
#8917 = CARTESIAN_POINT ( 'NONE',  ( 4.112796336321225432, 1.747692466664665600, -0.7127836182515898678 ) ) ;
#8918 = VERTEX_POINT ( 'NONE', #7460 ) ;
#8919 = ORIENTED_EDGE ( 'NONE', *, *, #8215, .F. ) ;
#8920 = AXIS2_PLACEMENT_3D ( 'NONE', #13971, #2515, #14135 ) ;
#8921 = ORIENTED_EDGE ( 'NONE', *, *, #9887, .T. ) ;
#8922 = DIRECTION ( 'NONE',  ( 0.000000000000000000, -2.708891287835076765E-14, -1.000000000000000000 ) ) ;
#8923 = VECTOR ( 'NONE', #387, 39.37007874015748143 ) ;
#8924 = VECTOR ( 'NONE', #750, 39.37007874015748143 ) ;
#8925 = CARTESIAN_POINT ( 'NONE',  ( 6.215861650065340527, 0.000000000000000000, 0.000000000000000000 ) ) ;
#8926 = DIRECTION ( 'NONE',  ( 0.000000000000000000, 0.000000000000000000, -1.000000000000000000 ) ) ;
#8927 = CARTESIAN_POINT ( 'NONE',  ( 6.826491571325181695, 1.679378605318035733, -1.304378605318064821 ) ) ;
#8928 = ORIENTED_EDGE ( 'NONE', *, *, #4468, .T. ) ;
#8929 = DIRECTION ( 'NONE',  ( 0.000000000000000000, 0.000000000000000000, 1.000000000000000000 ) ) ;
#8930 = DIRECTION ( 'NONE',  ( -0.7071067811865557884, 8.659560562354830553E-17, -0.7071067811865392461 ) ) ;
#8931 = DIRECTION ( 'NONE',  ( 0.7071067811865479058, 8.659560562354930393E-17, 0.7071067811865472397 ) ) ;
#8932 = CARTESIAN_POINT ( 'NONE',  ( 3.875000000000000000, 3.535499999999999865, -0.4849999999999995981 ) ) ;
#8933 = CONICAL_SURFACE ( 'NONE', #7235, 0.4849999999999995981, 0.7853981633974598253 ) ;
#8934 = DIRECTION ( 'NONE',  ( 0.000000000000000000, 1.000000000000000000, 0.000000000000000000 ) ) ;
#8935 = AXIS2_PLACEMENT_3D ( 'NONE', #8721, #10030, #14450 ) ;
#8936 = CONICAL_SURFACE ( 'NONE', #8460, 0.3750000000000004996, 0.7853981633974589371 ) ;
#8937 = CARTESIAN_POINT ( 'NONE',  ( 3.874999999999999556, 3.137999999999999901, 1.320000000000000062 ) ) ;
#8938 = B_SPLINE_CURVE_WITH_KNOTS ( 'NONE', 3,
 ( #920, #3312, #12333, #838, #7750, #14860, #9057, #2153, #13544, #4461 ),
 .UNSPECIFIED., .F., .F.,
 ( 4, 2, 2, 2, 4 ),
 ( 0.000000000000000000, 0.0002748923109770301477, 0.0005497846219540602954, 0.0008246769329310904431, 0.001099569243908120591 ),
 .UNSPECIFIED. ) ;
#8939 = CARTESIAN_POINT ( 'NONE',  ( 4.493377435082127391, 1.710570970923634526, 0.5097722557665413934 ) ) ;
#8940 = EDGE_CURVE ( 'NONE', #12407, #5002, #6534, .T. ) ;
#8942 = ORIENTED_EDGE ( 'NONE', *, *, #12317, .T. ) ;
#8941 = DIRECTION ( 'NONE',  ( -0.000000000000000000, -1.000000000000000000, -0.000000000000000000 ) ) ;
#8943 = ORIENTED_EDGE ( 'NONE', *, *, #3103, .T. ) ;
#8944 = EDGE_CURVE ( 'NONE', #11673, #8382, #5013, .T. ) ;
#8946 = ORIENTED_EDGE ( 'NONE', *, *, #1785, .T. ) ;
#8945 = DIRECTION ( 'NONE',  ( 0.000000000000000000, -0.000000000000000000, 1.000000000000000000 ) ) ;
#8947 = VERTEX_POINT ( 'NONE', #13029 ) ;
#8948 = DIRECTION ( 'NONE',  ( -0.01412288512831212997, 0.000000000000000000, 0.9999002670844990837 ) ) ;
#8949 = DIRECTION ( 'NONE',  ( 1.365923996832131609E-16, -1.000000000000000000, -0.000000000000000000 ) ) ;
#8950 = SHAPE_REPRESENTATION ( 'Lock Lever', ( #8424 ), #3023 ) ;
#8951 = ORIENTED_EDGE ( 'NONE', *, *, #2361, .T. ) ;
#8952 = CARTESIAN_POINT ( 'NONE',  ( 0.007060738305901492935, -0.2214999999999999469, 0.4999002720578262782 ) ) ;
#8953 = DIRECTION ( 'NONE',  ( 0.000000000000000000, -1.000000000000000000, -9.182682331643740718E-16 ) ) ;
#8954 = AXIS2_PLACEMENT_3D ( 'NONE', #11926, #10707, #8420 ) ;
#8955 = VECTOR ( 'NONE', #2719, 39.37007874015748854 ) ;
#8956 = EDGE_CURVE ( 'NONE', #8206, #3175, #6097, .T. ) ;
#8957 = CARTESIAN_POINT ( 'NONE',  ( 3.602264755523621353, 0.9969999999999997753, -0.4491205543005138412 ) ) ;
#8958 = CARTESIAN_POINT ( 'NONE',  ( 1.000000000000000222, -0.4429999999999998939, -0.3182109165419976238 ) ) ;
#8959 = VERTEX_POINT ( 'NONE', #9613 ) ;
#8960 = CIRCLE ( 'NONE', #3589, 0.07000000000000047851 ) ;
#8961 = CARTESIAN_POINT ( 'NONE',  ( 0.007060738305901492935, -0.2214999999999999469, 0.4999002720578262782 ) ) ;
#8962 = DIRECTION ( 'NONE',  ( 0.000000000000000000, 0.000000000000000000, -1.000000000000000000 ) ) ;
#8963 = EDGE_CURVE ( 'NONE', #14441, #13413, #10870, .T. ) ;
#8964 = CARTESIAN_POINT ( 'NONE',  ( 2.743000000000000327, 1.679378605318042395, -1.941878605318058115 ) ) ;
#8965 = EDGE_CURVE ( 'NONE', #14179, #13688, #6769, .T. ) ;
#8966 = CARTESIAN_POINT ( 'NONE',  ( 3.908596656942878500, 0.8665166726997025615, -0.4991519185931051483 ) ) ;
#8967 = VECTOR ( 'NONE', #7775, 39.37007874015748143 ) ;
#8968 = DIRECTION ( 'NONE',  ( -0.000000000000000000, -1.000000000000000000, -0.000000000000000000 ) ) ;
#8969 = VERTEX_POINT ( 'NONE', #6689 ) ;
#8970 = CARTESIAN_POINT ( 'NONE',  ( 0.000000000000000000, 0.000000000000000000, 0.000000000000000000 ) ) ;
#8971 = VERTEX_POINT ( 'NONE', #6621 ) ;
#8972 = SURFACE_STYLE_USAGE ( .BOTH. , #6446 ) ;
#8973 = ADVANCED_FACE ( 'NONE', ( #11197 ), #5547, .F. ) ;
#8974 = CIRCLE ( 'NONE', #7996, 0.2944999999999856066 ) ;
#8975 = CARTESIAN_POINT ( 'NONE',  ( 2.644772327656221833, 0.4573506435465171105, -0.4626444586489234512 ) ) ;
#8976 = DIRECTION ( 'NONE',  ( 0.000000000000000000, 0.000000000000000000, 1.000000000000000000 ) ) ;
#8977 = ADVANCED_FACE ( 'NONE', ( #5467 ), #1778, .F. ) ;
#8978 = FACE_OUTER_BOUND ( 'NONE', #15033, .T. ) ;
#8979 = FACE_OUTER_BOUND ( 'NONE', #4540, .T. ) ;
#8980 = CIRCLE ( 'NONE', #12873, 2.500000000000000000 ) ;
#8981 = LINE ( 'NONE', #7824, #13146 ) ;
#8982 = EDGE_CURVE ( 'NONE', #1773, #626, #6228, .T. ) ;
#8983 = ORIENTED_EDGE ( 'NONE', *, *, #10169, .T. ) ;
#8984 = DIRECTION ( 'NONE',  ( 0.000000000000000000, 0.000000000000000000, -1.000000000000000000 ) ) ;
#8985 = CYLINDRICAL_SURFACE ( 'NONE', #5205, 0.3750000000000004996 ) ;
#8986 = VECTOR ( 'NONE', #5020, 39.37007874015748143 ) ;
#8987 = DIRECTION ( 'NONE',  ( -0.000000000000000000, 1.000000000000000000, -0.000000000000000000 ) ) ;
#8988 = ORIENTED_EDGE ( 'NONE', *, *, #11960, .F. ) ;
#8989 = ORIENTED_EDGE ( 'NONE', *, *, #2103, .T. ) ;
#8990 = CARTESIAN_POINT ( 'NONE',  ( 1.569329279054357151, -0.05999999999999996309, 0.4778343322167462603 ) ) ;
#8991 = VERTEX_POINT ( 'NONE', #702 ) ;
#8992 = CARTESIAN_POINT ( 'NONE',  ( -0.3725000000000002198, -0.6290000000000005587, -0.4125000000000000333 ) ) ;
#8993 = VECTOR ( 'NONE', #7702, 39.37007874015748143 ) ;
#8994 = EDGE_CURVE ( 'NONE', #282, #11902, #13474, .T. ) ;
#8995 = CARTESIAN_POINT ( 'NONE',  ( 0.6746193685512168470, -0.3871368118416071424, -0.4906972545532032326 ) ) ;
#8996 = CARTESIAN_POINT ( 'NONE',  ( -5.764454660286586870E-18, 0.2159999999999999420, 0.000000000000000000 ) ) ;
#8997 = CARTESIAN_POINT ( 'NONE',  ( 3.876560711617219823, 1.855806856933289506, -0.7500000000000001110 ) ) ;
#8998 = EDGE_CURVE ( 'NONE', #969, #8382, #621, .T. ) ;
#8999 = ORIENTED_EDGE ( 'NONE', *, *, #13788, .T. ) ;
#9000 = FACE_OUTER_BOUND ( 'NONE', #11235, .T. ) ;
#9001 = CIRCLE ( 'NONE', #4355, 1.000000000000000222 ) ;
#9002 = ORIENTED_EDGE ( 'NONE', *, *, #12582, .T. ) ;
#9003 = CIRCLE ( 'NONE', #2404, 1.000000000000000000 ) ;
#9004 = ORIENTED_EDGE ( 'NONE', *, *, #4750, .F. ) ;
#9005 = VERTEX_POINT ( 'NONE', #11345 ) ;
#9006 = CARTESIAN_POINT ( 'NONE',  ( 3.874999999999999556, 3.105999999999998984, -1.320000000000000062 ) ) ;
#9007 = DIRECTION ( 'NONE',  ( 1.000000000000000000, 0.000000000000000000, 0.000000000000000000 ) ) ;
#9009 = CARTESIAN_POINT ( 'NONE',  ( 0.7810927279646683319, -0.4443615595214102099, -0.3417200794260679131 ) ) ;
#9008 = AXIS2_PLACEMENT_3D ( 'NONE', #12458, #1974, #11311 ) ;
#9010 = CONTEXT_DEPENDENT_SHAPE_REPRESENTATION ( #12503, #13608 ) ;
#9011 = DIRECTION ( 'NONE',  ( -1.000000000000000000, 0.000000000000000000, -0.000000000000000000 ) ) ;
#9012 = ORIENTED_EDGE ( 'NONE', *, *, #10910, .F. ) ;
#9013 = FACE_OUTER_BOUND ( 'NONE', #7864, .T. ) ;
#9014 = CARTESIAN_POINT ( 'NONE',  ( 1.000048944713735732, -0.4428998280398802612, -0.4293350073753851581 ) ) ;
#9015 = AXIS2_PLACEMENT_3D ( 'NONE', #10198, #13696, #12546 ) ;
#9016 = CIRCLE ( 'NONE', #4863, 0.2624999999999994560 ) ;
#9017 = CIRCLE ( 'NONE', #1175, 1.000000000000000000 ) ;
#9018 = EDGE_CURVE ( 'NONE', #2536, #4313, #14718, .T. ) ;
#9019 = CIRCLE ( 'NONE', #6571, 0.7849999999999969225 ) ;
#9020 = DIRECTION ( 'NONE',  ( -0.000000000000000000, -1.000000000000000000, -0.000000000000000000 ) ) ;
#9021 = AXIS2_PLACEMENT_3D ( 'NONE', #10214, #854, #9221 ) ;
#9022 = CARTESIAN_POINT ( 'NONE',  ( 4.417271851176087338, 1.781894997211476595, 0.5209725003072935845 ) ) ;
#9024 = ORIENTED_EDGE ( 'NONE', *, *, #2507, .F. ) ;
#9023 = CYLINDRICAL_SURFACE ( 'NONE', #11309, 3.000000000000000444 ) ;
#9025 = EDGE_LOOP ( 'NONE', ( #14023, #3346 ) ) ;
#9027 = VERTEX_POINT ( 'NONE', #2001 ) ;
#9026 = DIRECTION ( 'NONE',  ( -1.000000000000000000, -0.000000000000000000, -0.000000000000000000 ) ) ;
#9028 = ORIENTED_EDGE ( 'NONE', *, *, #10356, .T. ) ;
#9029 = CARTESIAN_POINT ( 'NONE',  ( 3.426491571325181340, 2.360000000000015863, 0.9799999999999454703 ) ) ;
#9030 = DIRECTION ( 'NONE',  ( 0.000000000000000000, 0.000000000000000000, -1.000000000000000000 ) ) ;
#9031 = VERTEX_POINT ( 'NONE', #2081 ) ;
#9032 = FACE_OUTER_BOUND ( 'NONE', #8597, .T. ) ;
#9033 = FACE_OUTER_BOUND ( 'NONE', #14750, .T. ) ;
#9034 = CONICAL_SURFACE ( 'NONE', #2434, 0.1899999999999996136, 0.7853981633974530530 ) ;
#9035 = CARTESIAN_POINT ( 'NONE',  ( 3.348322488999905477, 0.9844945895120515988, -0.4527073094774025086 ) ) ;
#9036 = CARTESIAN_POINT ( 'NONE',  ( 0.9751447534947045304, -0.4829432260179055136, -0.3788763210631934664 ) ) ;
#9037 = ORIENTED_EDGE ( 'NONE', *, *, #8325, .T. ) ;
#9038 = DIRECTION ( 'NONE',  ( 1.000000000000000000, 0.000000000000000000, -1.224646799147353207E-16 ) ) ;
#9039 = CARTESIAN_POINT ( 'NONE',  ( 3.379153571854337290, 0.9979286535324267682, 0.06644718038637786872 ) ) ;
#9040 = CARTESIAN_POINT ( 'NONE',  ( 2.774999999999999911, 0.000000000000000000, 0.000000000000000000 ) ) ;
#9041 = AXIS2_PLACEMENT_3D ( 'NONE', #5817, #1128, #12689 ) ;
#9042 = CARTESIAN_POINT ( 'NONE',  ( -0.2100000000000000200, 1.559103846021539619, -0.3809527529760087239 ) ) ;
#9043 = LINE ( 'NONE', #15076, #4549 ) ;
#9044 = ORIENTED_EDGE ( 'NONE', *, *, #8122, .F. ) ;
#9045 = DIRECTION ( 'NONE',  ( 0.000000000000000000, 0.000000000000000000, -1.000000000000000000 ) ) ;
#9046 = VERTEX_POINT ( 'NONE', #6463 ) ;
#9047 = DIRECTION ( 'NONE',  ( -0.000000000000000000, -0.000000000000000000, -1.000000000000000000 ) ) ;
#9048 = EDGE_CURVE ( 'NONE', #12391, #4893, #8909, .T. ) ;
#9049 = VECTOR ( 'NONE', #10849, 39.37007874015748143 ) ;
#9050 = EDGE_CURVE ( 'NONE', #4182, #6222, #1076, .T. ) ;
#9051 = CARTESIAN_POINT ( 'NONE',  ( 0.6866570596051723152, -0.4820476896543666179, -0.4282026755330073375 ) ) ;
#9052 = CARTESIAN_POINT ( 'NONE',  ( 0.4425000000000003375, 0.2159999999999999420, 0.3724999999999999423 ) ) ;
#9053 = EDGE_CURVE ( 'NONE', #355, #843, #9655, .T. ) ;
#9054 = CARTESIAN_POINT ( 'NONE',  ( 2.124999999999999556, 1.575000000000016387, 2.359999999999999876 ) ) ;
#9055 = ORIENTED_EDGE ( 'NONE', *, *, #6722, .F. ) ;
#9056 = FACE_OUTER_BOUND ( 'NONE', #2313, .T. ) ;
#9057 = CARTESIAN_POINT ( 'NONE',  ( 0.8282255603916048869, -0.4835890072320069843, -0.3529491429379406631 ) ) ;
#9058 = EDGE_CURVE ( 'NONE', #11308, #11151, #566, .T. ) ;
#9059 = PLANE ( 'NONE',  #8221 ) ;
#9060 = ORIENTED_EDGE ( 'NONE', *, *, #14038, .F. ) ;
#9061 = ORIENTED_EDGE ( 'NONE', *, *, #2217, .T. ) ;
#9062 = DIRECTION ( 'NONE',  ( -1.000000000000000000, -0.000000000000000000, -0.000000000000000000 ) ) ;
#9063 = CARTESIAN_POINT ( 'NONE',  ( -5.764454660286586870E-18, 0.2159999999999999420, 0.000000000000000000 ) ) ;
#9064 = ORIENTED_EDGE ( 'NONE', *, *, #8965, .T. ) ;
#9065 = DIRECTION ( 'NONE',  ( 0.000000000000000000, 0.000000000000000000, -1.000000000000000000 ) ) ;
#9066 = CARTESIAN_POINT ( 'NONE',  ( 0.7050899422473165812, -0.4211548882865318033, -0.4765263839844885996 ) ) ;
#9067 = CARTESIAN_POINT ( 'NONE',  ( 0.9445547394994807666, -0.4333281022995865706, -0.4594661707618462598 ) ) ;
#9068 = CARTESIAN_POINT ( 'NONE',  ( 4.181409934972732501, 1.788377768215813290, -0.6853619333027108906 ) ) ;
#9069 = VERTEX_POINT ( 'NONE', #8992 ) ;
#9070 = CARTESIAN_POINT ( 'NONE',  ( 3.791764282008899034, 1.827098821033795506, -0.7462103624669557123 ) ) ;
#9071 = ORIENTED_EDGE ( 'NONE', *, *, #5236, .F. ) ;
#9072 = EDGE_LOOP ( 'NONE', ( #8708, #4237, #7525, #4353 ) ) ;
#9073 = EDGE_CURVE ( 'NONE', #7551, #7643, #14791, .T. ) ;
#9074 = UNCERTAINTY_MEASURE_WITH_UNIT (LENGTH_MEASURE( 1.000000000000000082E-05 ), #5199, 'distance_accuracy_value', 'NONE');
#9075 = DIRECTION ( 'NONE',  ( 0.000000000000000000, 0.000000000000000000, -1.000000000000000000 ) ) ;
#9076 = ORIENTED_EDGE ( 'NONE', *, *, #1734, .F. ) ;
#9077 = CIRCLE ( 'NONE', #2236, 0.4070000000000022489 ) ;
#9078 = CARTESIAN_POINT ( 'NONE',  ( 2.774999999999999911, -2.360000000000016751, -1.574999999999999956 ) ) ;
#9079 = DIRECTION ( 'NONE',  ( 0.000000000000000000, 0.000000000000000000, -1.000000000000000000 ) ) ;
#9080 = CARTESIAN_POINT ( 'NONE',  ( 0.7818484599429001980, -0.4435097816930692605, -0.3509885469871208974 ) ) ;
#9081 = EDGE_CURVE ( 'NONE', #14657, #5216, #4323, .T. ) ;
#9082 = CARTESIAN_POINT ( 'NONE',  ( 0.09067304051454581904, 1.599165379501958473, -0.3809527529760087239 ) ) ;
#9083 = ORIENTED_EDGE ( 'NONE', *, *, #13412, .F. ) ;
#9084 = CARTESIAN_POINT ( 'NONE',  ( 3.153353529948859979, 2.492085072729484985, -0.2007741482994705173 ) ) ;
#9085 = DIRECTION ( 'NONE',  ( -1.000000000000000000, -0.000000000000000000, -0.000000000000000000 ) ) ;
#9086 = LENGTH_MEASURE_WITH_UNIT ( LENGTH_MEASURE( 0.02539999999999999897 ), #7934 );
#9087 = AXIS2_PLACEMENT_3D ( 'NONE', #3872, #7324, #13184 ) ;
#9088 = DIRECTION ( 'NONE',  ( 0.000000000000000000, 0.000000000000000000, -1.000000000000000000 ) ) ;
#9089 = CARTESIAN_POINT ( 'NONE',  ( 4.247233213520271278, 1.782208133480085444, 0.6529803701610973343 ) ) ;
#9091 = ORIENTED_EDGE ( 'NONE', *, *, #1243, .F. ) ;
#9090 = CARTESIAN_POINT ( 'NONE',  ( 3.426491571325181340, 2.058905028113295455, -0.2209981660730358233 ) ) ;
#9092 = VERTEX_POINT ( 'NONE', #12486 ) ;
#9094 = ORIENTED_EDGE ( 'NONE', *, *, #8154, .T. ) ;
#9093 = DIRECTION ( 'NONE',  ( 0.000000000000000000, 0.000000000000000000, -1.000000000000000000 ) ) ;
#9095 = VERTEX_POINT ( 'NONE', #10210 ) ;
#9096 = EDGE_CURVE ( 'NONE', #906, #4007, #14505, .T. ) ;
#9097 = DIRECTION ( 'NONE',  ( 0.000000000000000000, 0.000000000000000000, -1.000000000000000000 ) ) ;
#9098 = EDGE_CURVE ( 'NONE', #8887, #8503, #8755, .T. ) ;
#9099 = DIRECTION ( 'NONE',  ( 0.000000000000000000, 0.000000000000000000, -1.000000000000000000 ) ) ;
#9100 = ORIENTED_EDGE ( 'NONE', *, *, #1551, .F. ) ;
#9101 = LINE ( 'NONE', #11389, #14781 ) ;
#9102 = LINE ( 'NONE', #8113, #12424 ) ;
#9103 = CARTESIAN_POINT ( 'NONE',  ( 3.426491571325181340, -1.679378605318059048, -1.941878605318027251 ) ) ;
#9104 = DIRECTION ( 'NONE',  ( 1.000000000000000000, 0.000000000000000000, 0.000000000000000000 ) ) ;
#9105 = CARTESIAN_POINT ( 'NONE',  ( 2.956986065683827825, 0.9548522091764033437, -0.3979556114001199796 ) ) ;
#9106 = CARTESIAN_POINT ( 'NONE',  ( 2.187203820042824542, 0.4712135623730921985, 0.4085020630706684974 ) ) ;
#9107 = CIRCLE ( 'NONE', #6922, 0.05999999999999994227 ) ;
#9108 = ORIENTED_EDGE ( 'NONE', *, *, #12989, .T. ) ;
#9109 = CYLINDRICAL_SURFACE ( 'NONE', #1173, 0.9499999999999992895 ) ;
#9110 = CARTESIAN_POINT ( 'NONE',  ( 3.694556218107261536, 1.926530614425350674, 0.4685710943906171155 ) ) ;
#9111 = CARTESIAN_POINT ( 'NONE',  ( 3.504671749944806791, 1.917033125073213995, -0.7259803644674921452 ) ) ;
#9112 = DIRECTION ( 'NONE',  ( 0.000000000000000000, -1.000000000000000000, 0.000000000000000000 ) ) ;
#9114 = EDGE_LOOP ( 'NONE', ( #2662, #15017 ) ) ;
#9113 = DIRECTION ( 'NONE',  ( 0.7071067811865436870, 0.000000000000000000, -0.7071067811865512365 ) ) ;
#9115 = ORIENTED_EDGE ( 'NONE', *, *, #11032, .F. ) ;
#9116 = FACE_OUTER_BOUND ( 'NONE', #5766, .T. ) ;
#9117 = ORIENTED_EDGE ( 'NONE', *, *, #1108, .F. ) ;
#9118 = EDGE_CURVE ( 'NONE', #8521, #6113, #7604, .T. ) ;
#9119 =( GEOMETRIC_REPRESENTATION_CONTEXT ( 3 ) GLOBAL_UNCERTAINTY_ASSIGNED_CONTEXT ( ( #13650 ) ) GLOBAL_UNIT_ASSIGNED_CONTEXT ( ( #9552, #6454, #9821 ) ) REPRESENTATION_CONTEXT ( 'NONE', 'WORKASPACE' ) );
#9120 = CARTESIAN_POINT ( 'NONE',  ( 3.113342878570759531, 0.6489923502455472448, -0.4560262305286361673 ) ) ;
#9121 = CARTESIAN_POINT ( 'NONE',  ( 1.886930864189484636, -0.2403504688573024906, 0.4733484341213513580 ) ) ;
#9122 = DIRECTION ( 'NONE',  ( 0.000000000000000000, 0.000000000000000000, -1.000000000000000000 ) ) ;
#9123 = LINE ( 'NONE', #3307, #13060 ) ;
#9124 = AXIS2_PLACEMENT_3D ( 'NONE', #6881, #1194, #15128 ) ;
#9125 = DIRECTION ( 'NONE',  ( -1.000000000000000000, -0.000000000000000000, -0.000000000000000000 ) ) ;
#9126 = ORIENTED_EDGE ( 'NONE', *, *, #2180, .T. ) ;
#9127 = DIRECTION ( 'NONE',  ( 0.000000000000000000, 0.000000000000000000, -1.000000000000000000 ) ) ;
#9128 = CARTESIAN_POINT ( 'NONE',  ( 3.944129661530210385, 1.867491090171841117, 0.4951980309903491473 ) ) ;
#9129 = ORIENTED_EDGE ( 'NONE', *, *, #9714, .T. ) ;
#9130 = CARTESIAN_POINT ( 'NONE',  ( 3.426491571325181340, -1.574999999999984190, 1.575000000000033040 ) ) ;
#9131 = VERTEX_POINT ( 'NONE', #9988 ) ;
#9132 = ADVANCED_FACE ( 'NONE', ( #6541 ), #2315, .F. ) ;
#9133 = FACE_OUTER_BOUND ( 'NONE', #4227, .T. ) ;
#9134 = EDGE_CURVE ( 'NONE', #8556, #909, #15011, .T. ) ;
#9135 = DIRECTION ( 'NONE',  ( 0.000000000000000000, 1.000000000000000000, -1.224646799147353207E-16 ) ) ;
#9136 = ORIENTED_EDGE ( 'NONE', *, *, #9895, .T. ) ;
#9137 = EDGE_CURVE ( 'NONE', #11724, #10975, #5984, .T. ) ;
#9138 = AXIS2_PLACEMENT_3D ( 'NONE', #13746, #4512, #4670 ) ;
#9139 = DIRECTION ( 'NONE',  ( 0.000000000000000000, 0.000000000000000000, -1.000000000000000000 ) ) ;
#9140 = AXIS2_PLACEMENT_3D ( 'NONE', #12178, #6377, #9884 ) ;
#9141 = CARTESIAN_POINT ( 'NONE',  ( 0.7013471289190510438, -0.4108388036608545679, -0.4834044059207726618 ) ) ;
#9142 = CARTESIAN_POINT ( 'NONE',  ( 0.8999999999999999112, -0.6230000000000016636, -0.3750000000000000555 ) ) ;
#9143 = ADVANCED_FACE ( 'NONE', ( #3693 ), #10139, .F. ) ;
#9144 = DIRECTION ( 'NONE',  ( 0.000000000000000000, 0.000000000000000000, 1.000000000000000000 ) ) ;
#9145 = AXIS2_PLACEMENT_3D ( 'NONE', #4748, #9423, #128 ) ;
#9146 = AXIS2_PLACEMENT_3D ( 'NONE', #7141, #2461, #9354 ) ;
#9147 = ORIENTED_EDGE ( 'NONE', *, *, #519, .T. ) ;
#9148 = ADVANCED_FACE ( 'NONE', ( #9217 ), #1294, .F. ) ;
#9149 = ORIENTED_EDGE ( 'NONE', *, *, #1090, .F. ) ;
#9150 = CARTESIAN_POINT ( 'NONE',  ( -0.2285287788938155373, 1.564783867144732499, -0.3660820499162559805 ) ) ;
#9151 = ORIENTED_EDGE ( 'NONE', *, *, #3163, .F. ) ;
#9152 = CARTESIAN_POINT ( 'NONE',  ( 0.000000000000000000, 4.529999999999999361, -0.4999999999999997224 ) ) ;
#9153 = DIRECTION ( 'NONE',  ( 1.224646799147353207E-16, 0.000000000000000000, -1.000000000000000000 ) ) ;
#9154 = PLANE ( 'NONE',  #208 ) ;
#9155 = VECTOR ( 'NONE', #2943, 39.37007874015748854 ) ;
#9156 = CARTESIAN_POINT ( 'NONE',  ( -0.2027934381167096622, 1.564766993392025407, 0.3809527529760086684 ) ) ;
#9157 = ORIENTED_EDGE ( 'NONE', *, *, #13842, .F. ) ;
#9158 = CARTESIAN_POINT ( 'NONE',  ( 3.874999999999999556, 3.137999999999999901, 1.542499999999999760 ) ) ;
#9159 = LINE ( 'NONE', #14225, #13131 ) ;
#9160 = CARTESIAN_POINT ( 'NONE',  ( 0.6734872051250744285, -0.02989652563654837669, -0.4827143163826136396 ) ) ;
#9161 = FILL_AREA_STYLE ('',( #721 ) ) ;
#9162 = ADVANCED_FACE ( 'NONE', ( #2613 ), #14679, .T. ) ;
#9163 = CYLINDRICAL_SURFACE ( 'NONE', #3493, 0.1899999999999996136 ) ;
#9164 = EDGE_CURVE ( 'NONE', #15007, #4210, #7928, .T. ) ;
#9165 = CIRCLE ( 'NONE', #4287, 0.7849999999999996980 ) ;
#9166 = CARTESIAN_POINT ( 'NONE',  ( 4.543042897114498935, 1.795394141601344140, -0.3444184755256189945 ) ) ;
#9168 = ORIENTED_EDGE ( 'NONE', *, *, #14249, .T. ) ;
#9167 = DIRECTION ( 'NONE',  ( 0.000000000000000000, -1.000000000000000000, 0.000000000000000000 ) ) ;
#9169 = AXIS2_PLACEMENT_3D ( 'NONE', #4457, #13695, #10274 ) ;
#9170 = ORIENTED_EDGE ( 'NONE', *, *, #307, .F. ) ;
#9172 = ORIENTED_EDGE ( 'NONE', *, *, #13698, .T. ) ;
#9171 = DIRECTION ( 'NONE',  ( -1.365923996832131609E-16, 1.000000000000000000, 0.000000000000000000 ) ) ;
#9173 = ORIENTED_EDGE ( 'NONE', *, *, #13476, .F. ) ;
#9174 = DIRECTION ( 'NONE',  ( -0.9999002670844989726, 3.570356213862801578E-15, -0.01412288512831216640 ) ) ;
#9175 = CARTESIAN_POINT ( 'NONE',  ( 2.156999999999998696, -1.679378605318059048, -1.679378605318041950 ) ) ;
#9176 = ORIENTED_EDGE ( 'NONE', *, *, #1743, .F. ) ;
#9177 = FACE_OUTER_BOUND ( 'NONE', #14696, .T. ) ;
#9178 = FACE_OUTER_BOUND ( 'NONE', #5474, .T. ) ;
#9179 = AXIS2_PLACEMENT_3D ( 'NONE', #4698, #13013, #6149 ) ;
#9180 = CARTESIAN_POINT ( 'NONE',  ( -0.3725000000000002198, -0.6590000000000000302, -0.4424999999999983391 ) ) ;
#9181 = AXIS2_PLACEMENT_3D ( 'NONE', #11660, #9374, #6926 ) ;
#9182 = AXIS2_PLACEMENT_3D ( 'NONE', #280, #5130, #209 ) ;
#9183 = DIRECTION ( 'NONE',  ( -0.7070715176384851919, -0.7070715176384786416, -0.009986885842350882656 ) ) ;
#9184 = EDGE_CURVE ( 'NONE', #11117, #8801, #10375, .T. ) ;
#9185 = CARTESIAN_POINT ( 'NONE',  ( 2.124999999999999556, -1.679378605318041950, 1.679378605318059048 ) ) ;
#9186 = EDGE_CURVE ( 'NONE', #3698, #12880, #139, .T. ) ;
#9187 = CARTESIAN_POINT ( 'NONE',  ( 1.250000000000000000, 0.000000000000000000, 0.5000000000000000000 ) ) ;
#9188 = CARTESIAN_POINT ( 'NONE',  ( 3.808939537174094614, 0.8679352962517474790, 0.4967345602555460204 ) ) ;
#9189 = CARTESIAN_POINT ( 'NONE',  ( 4.064258325158515817, 1.735762175202256730, -0.7723679876275294509 ) ) ;
#9190 = VECTOR ( 'NONE', #7420, 39.37007874015748143 ) ;
#9191 = CARTESIAN_POINT ( 'NONE',  ( 3.944129661530210385, 0.000000000000000000, 0.000000000000000000 ) ) ;
#9193 = ORIENTED_EDGE ( 'NONE', *, *, #896, .F. ) ;
#9192 = FACE_OUTER_BOUND ( 'NONE', #780, .T. ) ;
#9194 = ORIENTED_EDGE ( 'NONE', *, *, #11893, .F. ) ;
#9195 = VECTOR ( 'NONE', #5901, 39.37007874015748143 ) ;
#9196 = AXIS2_PLACEMENT_3D ( 'NONE', #13719, #8793, #502 ) ;
#9197 = CARTESIAN_POINT ( 'NONE',  ( -0.2849999999999999201, 0.000000000000000000, 0.4108223460329290533 ) ) ;
#9198 = VERTEX_POINT ( 'NONE', #11794 ) ;
#9199 = FACE_OUTER_BOUND ( 'NONE', #11186, .T. ) ;
#9200 = APPLICATION_CONTEXT ( 'automotive_design' ) ;
#9201 = CARTESIAN_POINT ( 'NONE',  ( 3.319863249854039022, 0.6888833692903484351, -0.3931858364370118819 ) ) ;
#9202 = AXIS2_PLACEMENT_3D ( 'NONE', #12449, #6577, #9093 ) ;
#9203 = CARTESIAN_POINT ( 'NONE',  ( 2.184227569363401233, 0.01449120636682154316, 0.4691493281163361395 ) ) ;
#9204 = LINE ( 'NONE', #6840, #7452 ) ;
#9205 = CARTESIAN_POINT ( 'NONE',  ( 8.800855648616872529, 0.9403204140914576126, 0.3156881446850350326 ) ) ;
#9206 = ORIENTED_EDGE ( 'NONE', *, *, #10876, .F. ) ;
#9207 = EDGE_CURVE ( 'NONE', #8150, #7356, #1319, .T. ) ;
#9208 = CARTESIAN_POINT ( 'NONE',  ( 0.7010945348274502109, -0.4463672506600663281, 0.4266201320538802744 ) ) ;
#9209 = DIRECTION ( 'NONE',  ( -1.000000000000000000, -0.000000000000000000, -0.000000000000000000 ) ) ;
#9210 = ORIENTED_EDGE ( 'NONE', *, *, #8134, .F. ) ;
#9211 = FACE_OUTER_BOUND ( 'NONE', #9486, .T. ) ;
#9212 = ORIENTED_EDGE ( 'NONE', *, *, #2870, .F. ) ;
#9213 = CARTESIAN_POINT ( 'NONE',  ( 2.774999999999999911, 3.360000000000016751, 0.9799999999999461364 ) ) ;
#9214 = AXIS2_PLACEMENT_3D ( 'NONE', #12435, #14807, #2097 ) ;
#9215 = DIRECTION ( 'NONE',  ( 0.000000000000000000, 0.000000000000000000, 1.000000000000000000 ) ) ;
#9216 = VERTEX_POINT ( 'NONE', #9508 ) ;
#9217 = FACE_OUTER_BOUND ( 'NONE', #6933, .T. ) ;
#9218 = CARTESIAN_POINT ( 'NONE',  ( 3.388933043275772494, 0.7513023213622327390, 0.4521337140780258279 ) ) ;
#9219 = AXIS2_PLACEMENT_3D ( 'NONE', #11915, #15135, #2360 ) ;
#9220 = FACE_OUTER_BOUND ( 'NONE', #10955, .T. ) ;
#9221 = DIRECTION ( 'NONE',  ( 0.000000000000000000, 0.000000000000000000, -1.000000000000000000 ) ) ;
#9222 = EDGE_CURVE ( 'NONE', #9230, #7567, #14517, .T. ) ;
#9223 = VECTOR ( 'NONE', #11134, 39.37007874015748854 ) ;
#9224 = CARTESIAN_POINT ( 'NONE',  ( 2.774999999999999911, 2.359999999999999876, -1.575000000000016831 ) ) ;
#9225 = CARTESIAN_POINT ( 'NONE',  ( 3.895163492705322028, 1.774102321666491511, -0.7976064256867293478 ) ) ;
#9226 = VERTEX_POINT ( 'NONE', #11159 ) ;
#9227 = VECTOR ( 'NONE', #6408, 39.37007874015748143 ) ;
#9228 = ORIENTED_EDGE ( 'NONE', *, *, #13258, .T. ) ;
#9229 = CARTESIAN_POINT ( 'NONE',  ( 3.426491571325181340, 1.954234464180151676, 0.6847610993685215863 ) ) ;
#9230 = VERTEX_POINT ( 'NONE', #10028 ) ;
#9231 = FACE_OUTER_BOUND ( 'NONE', #14069, .T. ) ;
#9232 = LINE ( 'NONE', #471, #1491 ) ;
#9233 = FACE_BOUND ( 'NONE', #4395, .T. ) ;
#9234 = DIRECTION ( 'NONE',  ( -1.000000000000000000, -0.000000000000000000, -0.000000000000000000 ) ) ;
#9235 = VERTEX_POINT ( 'NONE', #659 ) ;
#9236 = CARTESIAN_POINT ( 'NONE',  ( 3.140023514803141680, 2.495986062540247019, -0.1444016757220298597 ) ) ;
#9237 = AXIS2_PLACEMENT_3D ( 'NONE', #5930, #8385, #13098 ) ;
#9238 = CARTESIAN_POINT ( 'NONE',  ( 0.6731911676472074335, -0.04506618701452713011, -0.4888638514297005688 ) ) ;
#9239 = CARTESIAN_POINT ( 'NONE',  ( -0.4125000000000000333, 0.1859999999999983611, 0.3724999999999999423 ) ) ;
#9240 = EDGE_CURVE ( 'NONE', #1703, #7368, #7216, .T. ) ;
#9241 = AXIS2_PLACEMENT_3D ( 'NONE', #2977, #14682, #1810 ) ;
#9242 = ADVANCED_FACE ( 'NONE', ( #12159 ), #4133, .T. ) ;
#9243 = EDGE_CURVE ( 'NONE', #5693, #1017, #10867, .T. ) ;
#9244 = SURFACE_STYLE_USAGE ( .BOTH. , #3580 ) ;
#9245 = VECTOR ( 'NONE', #3873, 39.37007874015748854 ) ;
#9246 = CARTESIAN_POINT ( 'NONE',  ( 4.616462829641571730, 1.747609168668489366, 0.1239280854323162873 ) ) ;
#9247 = VERTEX_POINT ( 'NONE', #5200 ) ;
#9249 = EDGE_LOOP ( 'NONE', ( #6338, #12638 ) ) ;
#9248 = DIRECTION ( 'NONE',  ( 0.000000000000000000, 0.000000000000000000, 1.000000000000000000 ) ) ;
#9250 = AXIS2_PLACEMENT_3D ( 'NONE', #12304, #13517, #2911 ) ;
#9251 = EDGE_CURVE ( 'NONE', #13964, #13774, #8437, .T. ) ;
#9252 = VERTEX_POINT ( 'NONE', #8872 ) ;
#9254 = ORIENTED_EDGE ( 'NONE', *, *, #9805, .F. ) ;
#9253 = LINE ( 'NONE', #38, #11397 ) ;
#9255 = ORIENTED_EDGE ( 'NONE', *, *, #14082, .F. ) ;
#9256 = EDGE_CURVE ( 'NONE', #2425, #3160, #6427, .T. ) ;
#9257 = FACE_OUTER_BOUND ( 'NONE', #10675, .T. ) ;
#9258 = CARTESIAN_POINT ( 'NONE',  ( 0.000000000000000000, 0.000000000000000000, 0.000000000000000000 ) ) ;
#9259 = ORIENTED_EDGE ( 'NONE', *, *, #3844, .F. ) ;
#9260 = VECTOR ( 'NONE', #2838, 39.37007874015748143 ) ;
#9261 = DIRECTION ( 'NONE',  ( 0.000000000000000000, 0.000000000000000000, -1.000000000000000000 ) ) ;
#9262 = CARTESIAN_POINT ( 'NONE',  ( 2.774999999999999911, 0.000000000000000000, 0.000000000000000000 ) ) ;
#9263 = AXIS2_PLACEMENT_3D ( 'NONE', #4149, #10187, #14838 ) ;
#9264 = DIRECTION ( 'NONE',  ( -0.000000000000000000, -1.000000000000000000, -0.000000000000000000 ) ) ;
#9265 = CIRCLE ( 'NONE', #4629, 0.1050000000000006622 ) ;
#9266 = CARTESIAN_POINT ( 'NONE',  ( -0.7287617923574203349, -0.6590000000000000302, -0.8499999999999999778 ) ) ;
#9267 = AXIS2_PLACEMENT_3D ( 'NONE', #4034, #9777, #8700 ) ;
#9268 = DIRECTION ( 'NONE',  ( 0.000000000000000000, 0.000000000000000000, -1.000000000000000000 ) ) ;
#9269 = CARTESIAN_POINT ( 'NONE',  ( 2.774999999999999911, -1.679378605318041950, 1.679378605318059048 ) ) ;
#9270 = CARTESIAN_POINT ( 'NONE',  ( 3.426491571325181340, -1.574999999999999956, 2.360000000000024745 ) ) ;
#9271 = VECTOR ( 'NONE', #7218, 39.37007874015748143 ) ;
#9272 = FACE_OUTER_BOUND ( 'NONE', #7831, .T. ) ;
#9273 = CARTESIAN_POINT ( 'NONE',  ( 0.000000000000000000, 4.529999999999999361, 0.000000000000000000 ) ) ;
#9274 = ADVANCED_FACE ( 'NONE', ( #6501 ), #1811, .T. ) ;
#9275 = CIRCLE ( 'NONE', #12429, 0.4070000000000058016 ) ;
#9276 = DIRECTION ( 'NONE',  ( -1.000000000000000000, -0.000000000000000000, -0.000000000000000000 ) ) ;
#9278 = ORIENTED_EDGE ( 'NONE', *, *, #8522, .T. ) ;
#9277 = FACE_BOUND ( 'NONE', #4562, .T. ) ;
#9279 = VERTEX_POINT ( 'NONE', #13217 ) ;
#9280 = EDGE_CURVE ( 'NONE', #7401, #11380, #330, .T. ) ;
#9281 = VECTOR ( 'NONE', #4488, 39.37007874015748854 ) ;
#9282 = DIRECTION ( 'NONE',  ( -0.000000000000000000, -1.000000000000000000, -0.000000000000000000 ) ) ;
#9283 = VECTOR ( 'NONE', #1797, 39.37007874015748143 ) ;
#9284 = ORIENTED_EDGE ( 'NONE', *, *, #12074, .T. ) ;
#9285 = CARTESIAN_POINT ( 'NONE',  ( 0.000000000000000000, 1.610000000000000098, 0.000000000000000000 ) ) ;
#9286 = ADVANCED_FACE ( 'NONE', ( #5358 ), #6284, .F. ) ;
#9287 = CARTESIAN_POINT ( 'NONE',  ( 2.738674485065001551, 0.4577639129046691124, -0.4613181569906135149 ) ) ;
#9288 = CARTESIAN_POINT ( 'NONE',  ( 0.8852856429364857060, 0.000000000000000000, -0.2372115730956926571 ) ) ;
#9289 = DIRECTION ( 'NONE',  ( -1.365923996832131609E-16, 1.000000000000000000, 0.000000000000000000 ) ) ;
#9290 = AXIS2_PLACEMENT_3D ( 'NONE', #10403, #9414, #49 ) ;
#9291 = ORIENTED_EDGE ( 'NONE', *, *, #3660, .T. ) ;
#9292 = CARTESIAN_POINT ( 'NONE',  ( 0.7051258599873114763, -0.4212171685758493433, 0.4764739269522876297 ) ) ;
#9293 = DIRECTION ( 'NONE',  ( -0.9999002670844991947, 2.602203049398214110E-17, 0.01412288512831213171 ) ) ;
#9294 = CARTESIAN_POINT ( 'NONE',  ( 6.794491571325179891, 1.679378605318035733, -1.304378605318064821 ) ) ;
#9295 = ORIENTED_EDGE ( 'NONE', *, *, #11949, .T. ) ;
#9296 = CARTESIAN_POINT ( 'NONE',  ( 3.390179639970223313, 0.6913388717410868800, 0.5000000000000000000 ) ) ;
#9297 = EDGE_LOOP ( 'NONE', ( #13336, #10612, #3976, #5874 ) ) ;
#9298 = CARTESIAN_POINT ( 'NONE',  ( 0.3724999999999997757, 0.2159999999999999420, -0.4425000000000005596 ) ) ;
#9299 = ORIENTED_EDGE ( 'NONE', *, *, #1136, .T. ) ;
#9300 = FACE_BOUND ( 'NONE', #7736, .T. ) ;
#9301 = AXIS2_PLACEMENT_3D ( 'NONE', #9639, #12068, #7197 ) ;
#9302 = EDGE_CURVE ( 'NONE', #14596, #12391, #12807, .T. ) ;
#9303 = DIRECTION ( 'NONE',  ( -0.000000000000000000, -1.000000000000000000, -0.000000000000000000 ) ) ;
#9304 = CYLINDRICAL_SURFACE ( 'NONE', #9728, 0.3750000000000004996 ) ;
#9305 = DIRECTION ( 'NONE',  ( 1.655665450705613915E-16, 0.000000000000000000, 1.000000000000000000 ) ) ;
#9306 = CARTESIAN_POINT ( 'NONE',  ( 3.912080264053299672, 1.844581235979443123, -0.7493606589675901875 ) ) ;
#9307 = ORIENTED_EDGE ( 'NONE', *, *, #1667, .F. ) ;
#9308 = ORIENTED_EDGE ( 'NONE', *, *, #14172, .F. ) ;
#9309 = CARTESIAN_POINT ( 'NONE',  ( 2.774999999999999911, -2.360000000000000320, 0.9799999999999999822 ) ) ;
#9310 = VERTEX_POINT ( 'NONE', #14375 ) ;
#9311 = DIRECTION ( 'NONE',  ( -0.3420201433256623846, 0.000000000000000000, 0.9396926207859106484 ) ) ;
#9312 = DIRECTION ( 'NONE',  ( -0.000000000000000000, 0.000000000000000000, 1.000000000000000000 ) ) ;
#9313 = CARTESIAN_POINT ( 'NONE',  ( 2.774999999999999911, 0.000000000000000000, 0.000000000000000000 ) ) ;
#9314 = ORIENTED_EDGE ( 'NONE', *, *, #1090, .T. ) ;
#9315 = AXIS2_PLACEMENT_3D ( 'NONE', #11684, #8174, #10380 ) ;
#9316 = EDGE_CURVE ( 'NONE', #10863, #3169, #14030, .T. ) ;
#9317 = CARTESIAN_POINT ( 'NONE',  ( 3.181442653385367247, 2.484069017451620898, -0.2831152458680617490 ) ) ;
#9318 = DIRECTION ( 'NONE',  ( -0.7070715176384847478, -0.7070715176384790857, 0.009986885842352487275 ) ) ;
#9319 = CARTESIAN_POINT ( 'NONE',  ( -5.764454660286586870E-18, 0.1759999999999999065, 0.000000000000000000 ) ) ;
#9320 = FACE_OUTER_BOUND ( 'NONE', #10040, .T. ) ;
#9321 = CIRCLE ( 'NONE', #5664, 0.5000000000000002220 ) ;
#9322 = CARTESIAN_POINT ( 'NONE',  ( 4.516637308352397184, 1.791637356194117681, -0.3913067716919665373 ) ) ;
#9323 = VERTEX_POINT ( 'NONE', #7573 ) ;
#9325 = ORIENTED_EDGE ( 'NONE', *, *, #2136, .T. ) ;
#9324 = DIRECTION ( 'NONE',  ( 0.000000000000000000, 0.000000000000000000, -1.000000000000000000 ) ) ;
#9326 = ORIENTED_EDGE ( 'NONE', *, *, #13787, .T. ) ;
#9328 = VERTEX_POINT ( 'NONE', #2754 ) ;
#9327 = CARTESIAN_POINT ( 'NONE',  ( 3.874999999999999556, 2.750000000000000000, 1.542000000000002258 ) ) ;
#9329 = EDGE_LOOP ( 'NONE', ( #536, #730, #8770, #6627 ) ) ;
#9330 = ADVANCED_FACE ( 'NONE', ( #12231 ), #7426, .F. ) ;
#9331 = EDGE_CURVE ( 'NONE', #15092, #2489, #9794, .T. ) ;
#9332 = DIRECTION ( 'NONE',  ( -0.000000000000000000, -0.000000000000000000, -1.000000000000000000 ) ) ;
#9333 = DIRECTION ( 'NONE',  ( 0.000000000000000000, 0.000000000000000000, 1.000000000000000000 ) ) ;
#9334 = CARTESIAN_POINT ( 'NONE',  ( 3.876560711617219379, 3.567999999999999616, 0.000000000000000000 ) ) ;
#9335 = ORIENTED_EDGE ( 'NONE', *, *, #617, .F. ) ;
#9336 = EDGE_CURVE ( 'NONE', #1080, #4626, #9896, .T. ) ;
#9337 = DIRECTION ( 'NONE',  ( -1.000000000000000000, -0.000000000000000000, -0.000000000000000000 ) ) ;
#9338 = CARTESIAN_POINT ( 'NONE',  ( 6.794491571325181667, 1.679378605318059492, 2.054378605318042172 ) ) ;
#9339 = CYLINDRICAL_SURFACE ( 'NONE', #5145, 1.500000000000000222 ) ;
#9340 = FACE_OUTER_BOUND ( 'NONE', #2234, .T. ) ;
#9341 = DIRECTION ( 'NONE',  ( -0.000000000000000000, -1.000000000000000000, -0.000000000000000000 ) ) ;
#9342 = EDGE_CURVE ( 'NONE', #1969, #13854, #12301, .T. ) ;
#9343 = DIRECTION ( 'NONE',  ( 1.000000000000000000, 0.000000000000000000, 0.000000000000000000 ) ) ;
#9344 = CARTESIAN_POINT ( 'NONE',  ( 5.546318247523970513, 0.000000000000000000, 0.000000000000000000 ) ) ;
#9345 = DIRECTION ( 'NONE',  ( -1.000000000000000000, 0.000000000000000000, 0.000000000000000000 ) ) ;
#9346 = CARTESIAN_POINT ( 'NONE',  ( 8.472944879060717582, 0.9288399267729603448, 0.3803256373014023417 ) ) ;
#9347 = CARTESIAN_POINT ( 'NONE',  ( 4.673606863172930836, 1.731232082755191914, -0.1365754461054935476 ) ) ;
#9348 = VERTEX_POINT ( 'NONE', #10318 ) ;
#9349 = DIRECTION ( 'NONE',  ( 0.7071067811865519026, 0.000000000000000000, -0.7071067811865430208 ) ) ;
#9351 = ORIENTED_EDGE ( 'NONE', *, *, #10964, .T. ) ;
#9350 = CARTESIAN_POINT ( 'NONE',  ( 6.794491571325181667, 1.679378605318059492, 2.054378605318042172 ) ) ;
#9352 = ORIENTED_EDGE ( 'NONE', *, *, #11669, .T. ) ;
#9353 = CARTESIAN_POINT ( 'NONE',  ( 0.09500000000000431710, 1.679378605318035733, -1.679378605318065487 ) ) ;
#9354 = DIRECTION ( 'NONE',  ( 0.000000000000000000, 0.000000000000000000, -1.000000000000000000 ) ) ;
#9355 = ORIENTED_EDGE ( 'NONE', *, *, #6913, .T. ) ;
#9356 = DIRECTION ( 'NONE',  ( 0.000000000000000000, 0.000000000000000000, -1.000000000000000000 ) ) ;
#9357 =( BOUNDED_SURFACE ( )  B_SPLINE_SURFACE ( 3, 2, ( 
 ( #2046, #6509, #5592 ),
 ( #12605, #6737, #8876 ),
 ( #4215, #897, #10255 ),
 ( #3144, #1976, #7807 ),
 ( #14913, #741, #7726 ),
 ( #9105, #10183, #12460 ),
 ( #3061, #4440, #10104 ),
 ( #13747, #3287, #9035 ),
 ( #5438, #11246, #7957 ),
 ( #4291, #13679, #8957 ) ),
 .UNSPECIFIED., .F., .F., .F. ) 
 B_SPLINE_SURFACE_WITH_KNOTS ( ( 4, 2, 2, 2, 4 ),
 ( 3, 3 ),
 ( 0.7853981633974462806, 0.9817477042468089055, 1.178097245096171530, 1.374446785945534044, 1.570796326794896558 ),
 ( 0.000000000000000000, 1.000000000000000000 ),
 .UNSPECIFIED. ) 
 GEOMETRIC_REPRESENTATION_ITEM ( )  RATIONAL_B_SPLINE_SURFACE ( (
 ( 1.000000000000000000, 0.7035672008258542220, 1.000000000000000000),
 ( 1.000000000000000000, 0.7037994241808144258, 1.000000000000000000),
 ( 1.000000000000000000, 0.7040544485617191706, 1.000000000000000000),
 ( 1.000000000000000000, 0.7046000480543618272, 1.000000000000000000),
 ( 1.000000000000000000, 0.7048906332660594964, 1.000000000000000000),
 ( 1.000000000000000000, 0.7054961263457840692, 1.000000000000000000),
 ( 1.000000000000000000, 0.7058110186534256592, 1.000000000000000000),
 ( 1.000000000000000000, 0.7064529522758904445, 1.000000000000000000),
 ( 1.000000000000000000, 0.7067799747760905582, 1.000000000000000000),
 ( 1.000000000000000000, 0.7071067811865475727, 1.000000000000000000) ) ) 
 REPRESENTATION_ITEM ( '' )  SURFACE ( )  );
#9358 = PLANE ( 'NONE',  #15026 ) ;
#9359 = DIRECTION ( 'NONE',  ( -0.000000000000000000, -1.000000000000000000, -0.000000000000000000 ) ) ;
#9360 = EDGE_CURVE ( 'NONE', #193, #14590, #11357, .T. ) ;
#9361 = ORIENTED_EDGE ( 'NONE', *, *, #8650, .F. ) ;
#9362 = CARTESIAN_POINT ( 'NONE',  ( 0.7026382878072456872, -0.3911443797526893973, 0.4896667335905586227 ) ) ;
#9363 = CARTESIAN_POINT ( 'NONE',  ( 0.6500000000000001332, 1.679378605318059492, 1.272378605318037037 ) ) ;
#9364 = CIRCLE ( 'NONE', #2758, 0.3750000000000007772 ) ;
#9365 = CARTESIAN_POINT ( 'NONE',  ( 4.315797241329101475, 2.750000000000000000, -1.570821732971949825 ) ) ;
#9366 = VERTEX_POINT ( 'NONE', #11387 ) ;
#9367 = EDGE_CURVE ( 'NONE', #9653, #9554, #8209, .T. ) ;
#9368 = DIRECTION ( 'NONE',  ( 0.000000000000000000, 0.000000000000000000, 1.000000000000000000 ) ) ;
#9369 = CARTESIAN_POINT ( 'NONE',  ( 2.774999999999999911, 0.7000000000000030642, 2.399999999999999911 ) ) ;
#9370 = ORIENTED_EDGE ( 'NONE', *, *, #7407, .F. ) ;
#9371 = AXIS2_PLACEMENT_3D ( 'NONE', #6876, #10236, #9088 ) ;
#9372 = CARTESIAN_POINT ( 'NONE',  ( 0.7727406610312560487, 0.000000000000000000, -0.2070552360820117899 ) ) ;
#9373 = ORIENTED_EDGE ( 'NONE', *, *, #10322, .F. ) ;
#9374 = DIRECTION ( 'NONE',  ( -0.2588190451025147443, 0.000000000000000000, -0.9659258262890698665 ) ) ;
#9375 = AXIS2_PLACEMENT_3D ( 'NONE', #10055, #7676, #613 ) ;
#9376 = LINE ( 'NONE', #11815, #4638 ) ;
#9377 = DIRECTION ( 'NONE',  ( 1.000000000000000000, 0.000000000000000000, 0.000000000000000000 ) ) ;
#9378 = CARTESIAN_POINT ( 'NONE',  ( 0.8999999999999998002, 0.000000000000000000, -0.3799999999999999489 ) ) ;
#9379 = EDGE_CURVE ( 'NONE', #4605, #10756, #8447, .T. ) ;
#9380 = EDGE_CURVE ( 'NONE', #11912, #14903, #14753, .T. ) ;
#9381 = CIRCLE ( 'NONE', #11818, 0.03999999999999998002 ) ;
#9382 = CARTESIAN_POINT ( 'NONE',  ( 3.818939198319201367, 1.796011530029135717, -0.7986547527183526229 ) ) ;
#9383 = ORIENTED_EDGE ( 'NONE', *, *, #13518, .T. ) ;
#9384 = ORIENTED_EDGE ( 'NONE', *, *, #3238, .F. ) ;
#9385 = VECTOR ( 'NONE', #4451, 39.37007874015748143 ) ;
#9386 = LINE ( 'NONE', #7101, #9445 ) ;
#9387 = EDGE_LOOP ( 'NONE', ( #10770, #4504, #1530, #14615 ) ) ;
#9388 = CARTESIAN_POINT ( 'NONE',  ( 0.3724999999999997757, 0.2159999999999999698, -0.4125000000000000333 ) ) ;
#9389 = FACE_OUTER_BOUND ( 'NONE', #11955, .T. ) ;
#9390 = DIRECTION ( 'NONE',  ( 1.000000000000000000, 0.000000000000000000, 0.000000000000000000 ) ) ;
#9391 = CYLINDRICAL_SURFACE ( 'NONE', #13858, 2.500000000000000444 ) ;
#9392 = ORIENTED_EDGE ( 'NONE', *, *, #13320, .T. ) ;
#9393 = CARTESIAN_POINT ( 'NONE',  ( 3.447448974675020317, 1.983204662126842655, -0.2635305192258420304 ) ) ;
#9394 = DIRECTION ( 'NONE',  ( -1.000000000000000000, -0.000000000000000000, -0.000000000000000000 ) ) ;
#9395 = VECTOR ( 'NONE', #8043, 39.37007874015748143 ) ;
#9396 = CYLINDRICAL_SURFACE ( 'NONE', #988, 0.2624999999999852451 ) ;
#9397 =( GEOMETRIC_REPRESENTATION_CONTEXT ( 3 ) GLOBAL_UNCERTAINTY_ASSIGNED_CONTEXT ( ( #14107 ) ) GLOBAL_UNIT_ASSIGNED_CONTEXT ( ( #1449, #2688, #14516 ) ) REPRESENTATION_CONTEXT ( 'NONE', 'WORKASPACE' ) );
#9398 = FACE_OUTER_BOUND ( 'NONE', #14431, .T. ) ;
#9399 = EDGE_CURVE ( 'NONE', #10976, #6033, #2071, .T. ) ;
#9400 = CARTESIAN_POINT ( 'NONE',  ( 4.602419216495897025, 1.720910125550154213, -0.3479222348275701204 ) ) ;
#9401 = EDGE_LOOP ( 'NONE', ( #9206, #3736 ) ) ;
#9403 = ORIENTED_EDGE ( 'NONE', *, *, #9784, .T. ) ;
#9402 = CARTESIAN_POINT ( 'NONE',  ( 0.3208174396730070210, 1.603403006623434601, 0.2062334004842066582 ) ) ;
#9404 = ORIENTED_EDGE ( 'NONE', *, *, #13318, .F. ) ;
#9405 = CIRCLE ( 'NONE', #7931, 2.500000000000000000 ) ;
#9406 = VERTEX_POINT ( 'NONE', #1971 ) ;
#9407 = EDGE_CURVE ( 'NONE', #259, #1274, #6024, .T. ) ;
#9408 = DIRECTION ( 'NONE',  ( 0.000000000000000000, 0.000000000000000000, 1.000000000000000000 ) ) ;
#9409 = SHAPE_REPRESENTATION_RELATIONSHIP ( 'NONE' , 'NONE' ,  #8950, #8388 ) ;
#9410 = CARTESIAN_POINT ( 'NONE',  ( 0.000000000000000000, 2.750000000000000000, 0.000000000000000000 ) ) ;
#9411 = ORIENTED_EDGE ( 'NONE', *, *, #9073, .F. ) ;
#9412 = LINE ( 'NONE', #10779, #3861 ) ;
#9413 = FACE_OUTER_BOUND ( 'NONE', #12595, .T. ) ;
#9414 = DIRECTION ( 'NONE',  ( -0.000000000000000000, -1.000000000000000000, -0.000000000000000000 ) ) ;
#9415 = FACE_OUTER_BOUND ( 'NONE', #9696, .T. ) ;
#9416 = AXIS2_PLACEMENT_3D ( 'NONE', #4245, #847, #7682 ) ;
#9417 = EDGE_CURVE ( 'NONE', #3160, #2506, #10881, .T. ) ;
#9418 = DIRECTION ( 'NONE',  ( -0.9999002670844990837, 5.351333901719070118E-15, 0.01412288512831215426 ) ) ;
#9419 = AXIS2_PLACEMENT_3D ( 'NONE', #1847, #11189, #8984 ) ;
#9420 = VECTOR ( 'NONE', #322, 39.37007874015748143 ) ;
#9421 = DIRECTION ( 'NONE',  ( 0.000000000000000000, 0.000000000000000000, 1.000000000000000000 ) ) ;
#9422 = DIRECTION ( 'NONE',  ( 0.000000000000000000, 0.000000000000000000, -1.000000000000000000 ) ) ;
#9423 = DIRECTION ( 'NONE',  ( -0.7070715176384830825, -0.7070715176384807510, 0.009986885842350853165 ) ) ;
#9424 = ORIENTED_EDGE ( 'NONE', *, *, #7782, .T. ) ;
#9425 = LINE ( 'NONE', #14920, #14536 ) ;
#9427 = EDGE_LOOP ( 'NONE', ( #4692, #9024, #13504, #8641 ) ) ;
#9426 = DIRECTION ( 'NONE',  ( 0.000000000000000000, 0.000000000000000000, -1.000000000000000000 ) ) ;
#9428 = ORIENTED_EDGE ( 'NONE', *, *, #8956, .F. ) ;
#9429 = CARTESIAN_POINT ( 'NONE',  ( 2.124999999999999556, 0.9799999999999438050, -2.360000000000016307 ) ) ;
#9430 = EDGE_CURVE ( 'NONE', #9069, #2309, #6808, .T. ) ;
#9431 = CARTESIAN_POINT ( 'NONE',  ( 3.426491571325181340, -3.000039370078740220, 0.5999481385559802815 ) ) ;
#9432 = ORIENTED_EDGE ( 'NONE', *, *, #7650, .T. ) ;
#9433 = CARTESIAN_POINT ( 'NONE',  ( 3.874999999999999556, 3.137999999999999901, 1.542499999999999760 ) ) ;
#9434 = AXIS2_PLACEMENT_3D ( 'NONE', #6903, #11787, #12844 ) ;
#9435 = CARTESIAN_POINT ( 'NONE',  ( 0.3724999999999999423, 0.2159999999999999420, 0.4425000000000003930 ) ) ;
#9436 = ADVANCED_FACE ( 'NONE', ( #10398 ), #1328, .F. ) ;
#9437 = CARTESIAN_POINT ( 'NONE',  ( 0.000000000000000000, 1.109999999999999876, -0.4850000000000000977 ) ) ;
#9438 = ORIENTED_EDGE ( 'NONE', *, *, #8216, .T. ) ;
#9439 = VECTOR ( 'NONE', #229, 39.37007874015748854 ) ;
#9440 = ADVANCED_FACE ( 'NONE', ( #4433 ), #5432, .F. ) ;
#9441 = LINE ( 'NONE', #14085, #13389 ) ;
#9442 = LINE ( 'NONE', #9594, #4966 ) ;
#9443 = CONICAL_SURFACE ( 'NONE', #4301, 0.1899999999999996136, 0.7853981633974530530 ) ;
#9444 = DIRECTION ( 'NONE',  ( 1.000000000000000000, 0.000000000000000000, 0.000000000000000000 ) ) ;
#9445 = VECTOR ( 'NONE', #4946, 39.37007874015748143 ) ;
#9446 = ORIENTED_EDGE ( 'NONE', *, *, #11513, .T. ) ;
#9447 = DIRECTION ( 'NONE',  ( -1.000000000000000000, -0.000000000000000000, -0.000000000000000000 ) ) ;
#9448 = ORIENTED_EDGE ( 'NONE', *, *, #12871, .T. ) ;
#9449 = EDGE_CURVE ( 'NONE', #6091, #3024, #344, .T. ) ;
#9450 = DIRECTION ( 'NONE',  ( 0.000000000000000000, 0.000000000000000000, 1.000000000000000000 ) ) ;
#9451 = EDGE_LOOP ( 'NONE', ( #11013, #13607, #2940, #14397 ) ) ;
#9452 = EDGE_CURVE ( 'NONE', #5573, #1719, #1086, .T. ) ;
#9453 = CARTESIAN_POINT ( 'NONE',  ( 0.000000000000000000, 1.377727649040773375E-16, -1.125000000000000888 ) ) ;
#9454 = CONICAL_SURFACE ( 'NONE', #5046, 0.3750000000000004996, 0.7853981633974547183 ) ;
#9455 = CARTESIAN_POINT ( 'NONE',  ( 1.625945750339073292, -0.2839166429012424109, -0.4770346645432335664 ) ) ;
#9456 = AXIS2_PLACEMENT_3D ( 'NONE', #14021, #10753, #12797 ) ;
#9457 = CIRCLE ( 'NONE', #13325, 0.2944999999999998175 ) ;
#9458 = FACE_OUTER_BOUND ( 'NONE', #2122, .T. ) ;
#9459 = DIRECTION ( 'NONE',  ( 1.000000000000000000, 0.000000000000000000, 0.000000000000000000 ) ) ;
#9460 = ORIENTED_EDGE ( 'NONE', *, *, #7924, .F. ) ;
#9461 = EDGE_LOOP ( 'NONE', ( #9766, #8890, #2158, #6134 ) ) ;
#9462 = ORIENTED_EDGE ( 'NONE', *, *, #9911, .F. ) ;
#9463 = EDGE_CURVE ( 'NONE', #13095, #12994, #6241, .T. ) ;
#9464 = DIRECTION ( 'NONE',  ( 1.000000000000000000, 0.000000000000000000, 0.000000000000000000 ) ) ;
#9465 = CARTESIAN_POINT ( 'NONE',  ( 0.6500000000000001332, 1.679378605318059492, 1.679378605318041506 ) ) ;
#9466 = CARTESIAN_POINT ( 'NONE',  ( 6.794491571325179891, -1.679378605318048390, 1.304378605318053497 ) ) ;
#9467 = DIRECTION ( 'NONE',  ( 0.000000000000000000, 0.7071067811865441310, 0.7071067811865509034 ) ) ;
#9468 = ORIENTED_EDGE ( 'NONE', *, *, #12348, .T. ) ;
#9469 = CARTESIAN_POINT ( 'NONE',  ( 2.156999999999999584, 1.679378605318059048, 1.679378605318041506 ) ) ;
#9470 = ADVANCED_FACE ( 'NONE', ( #4357 ), #7872, .T. ) ;
#9471 = CIRCLE ( 'NONE', #8484, 1.000000000000000000 ) ;
#9472 = CARTESIAN_POINT ( 'NONE',  ( 1.844710921988372831, 0.09661955516503824282, 0.4739447609888647328 ) ) ;
#9473 = DIRECTION ( 'NONE',  ( 0.5000000000000101030, 0.000000000000000000, 0.8660254037844328234 ) ) ;
#9474 = CIRCLE ( 'NONE', #4589, 0.7173254825712085392 ) ;
#9475 = CARTESIAN_POINT ( 'NONE',  ( 3.876560711617219379, 2.749999999999999556, -0.7500000000000001110 ) ) ;
#9476 = CARTESIAN_POINT ( 'NONE',  ( 4.544715742067830355, 1.738214473614324573, -0.3411839755103457383 ) ) ;
#9477 = ORIENTED_EDGE ( 'NONE', *, *, #916, .T. ) ;
#9479 = ORIENTED_EDGE ( 'NONE', *, *, #12325, .T. ) ;
#9478 = CARTESIAN_POINT ( 'NONE',  ( 0.4273790000700227187, 1.569549437900746636, 0.02166336374275166718 ) ) ;
#9480 = ORIENTED_EDGE ( 'NONE', *, *, #13547, .T. ) ;
#9481 = CYLINDRICAL_SURFACE ( 'NONE', #381, 0.1900000000000000577 ) ;
#9482 = EDGE_LOOP ( 'NONE', ( #4407, #9392, #8095, #7600 ) ) ;
#9483 = CARTESIAN_POINT ( 'NONE',  ( 3.874999999999999556, 3.137999999999999901, -1.320000000000000062 ) ) ;
#9484 = APPLICATION_PROTOCOL_DEFINITION ( 'draft international standard', 'automotive_design', 1998, #8616 ) ;
#9485 = PLANE ( 'NONE',  #6734 ) ;
#9486 = EDGE_LOOP ( 'NONE', ( #8145, #5348, #8593, #15131 ) ) ;
#9487 = DIRECTION ( 'NONE',  ( 0.000000000000000000, 0.000000000000000000, -1.000000000000000000 ) ) ;
#9488 = CYLINDRICAL_SURFACE ( 'NONE', #201, 0.3750000000000004996 ) ;
#9489 = AXIS2_PLACEMENT_3D ( 'NONE', #284, #7140, #13994 ) ;
#9490 = B_SPLINE_CURVE_WITH_KNOTS ( 'NONE', 3,
 ( #13594, #7342, #4901, #10702, #195, #3509, #1503, #119, #11920, #1204, #4819, #11703, #8190, #5896 ),
 .UNSPECIFIED., .F., .F.,
 ( 4, 2, 2, 2, 2, 2, 4 ),
 ( 0.02339532894303463992, 0.02409265248687550084, 0.02478997603071635830, 0.02618462311839807322, 0.02757927020607978813, 0.02827659374992064559, 0.02897391729376150304 ),
 .UNSPECIFIED. ) ;
#9491 = EDGE_CURVE ( 'NONE', #13193, #4331, #9165, .T. ) ;
#9492 = CARTESIAN_POINT ( 'NONE',  ( 3.675055934133140578, 1.933571379205582863, 0.7235290732629748867 ) ) ;
#9493 = CARTESIAN_POINT ( 'NONE',  ( 0.1807106342563528367, 1.379999999999999671, 5.178337979384803075E-18 ) ) ;
#9494 = PRODUCT_RELATED_PRODUCT_CATEGORY ( 'part', '', ( #12392 ) ) ;
#9495 = AXIS2_PLACEMENT_3D ( 'NONE', #1697, #11033, #5384 ) ;
#9496 = CARTESIAN_POINT ( 'NONE',  ( 3.426491571325181340, 0.000000000000000000, 0.000000000000000000 ) ) ;
#9497 = CARTESIAN_POINT ( 'NONE',  ( 3.469399777640902460, 0.9562660893803829332, 0.2928328421798268022 ) ) ;
#9498 = VECTOR ( 'NONE', #1892, 39.37007874015748854 ) ;
#9499 = DIRECTION ( 'NONE',  ( 0.000000000000000000, -0.000000000000000000, -1.000000000000000000 ) ) ;
#9500 = ORIENTED_EDGE ( 'NONE', *, *, #9342, .F. ) ;
#9501 = CARTESIAN_POINT ( 'NONE',  ( 6.794491571325181667, 1.679378605318059492, 1.679378605318041506 ) ) ;
#9503 = ORIENTED_EDGE ( 'NONE', *, *, #3999, .T. ) ;
#9502 = FACE_OUTER_BOUND ( 'NONE', #6116, .T. ) ;
#9504 = ORIENTED_EDGE ( 'NONE', *, *, #6508, .T. ) ;
#9505 = VECTOR ( 'NONE', #7298, 39.37007874015748854 ) ;
#9506 = DIRECTION ( 'NONE',  ( 0.000000000000000000, 0.000000000000000000, 1.000000000000000000 ) ) ;
#9507 = CARTESIAN_POINT ( 'NONE',  ( -0.3725000000000000533, 0.2159999999999999420, 0.3724999999999999423 ) ) ;
#9508 = CARTESIAN_POINT ( 'NONE',  ( 2.592367411162173507, 0.4049457270506671147, 0.4633846410852800468 ) ) ;
#9509 = ORIENTED_EDGE ( 'NONE', *, *, #11199, .T. ) ;
#9510 = CARTESIAN_POINT ( 'NONE',  ( 3.875000000000000000, 1.112678268764263789, 0.000000000000000000 ) ) ;
#9511 = CIRCLE ( 'NONE', #11446, 0.3750000000000007772 ) ;
#9512 = LINE ( 'NONE', #10651, #2806 ) ;
#9513 =( BOUNDED_SURFACE ( )  B_SPLINE_SURFACE ( 3, 2, ( 
 ( #607, #13467, #3004 ),
 ( #12328, #1843, #6529 ),
 ( #11185, #687, #5385 ),
 ( #758, #5458, #14162 ) ),
 .UNSPECIFIED., .F., .F., .F. ) 
 B_SPLINE_SURFACE_WITH_KNOTS ( ( 4, 4 ),
 ( 3, 3 ),
 ( -3.252606517456513302E-18, 0.0001672156045178513220 ),
 ( 0.000000000000000000, 1.000000000000000000 ),
 .UNSPECIFIED. ) 
 GEOMETRIC_REPRESENTATION_ITEM ( )  RATIONAL_B_SPLINE_SURFACE ( (
 ( 1.000000000000000000, 0.7075975758264662074, 1.000000000000000000),
 ( 1.000000000000000000, 0.7105806483792744821, 1.000000000000000000),
 ( 1.000000000000000000, 0.7138423292275878351, 1.000000000000000000),
 ( 1.000000000000000000, 0.7173416231802122178, 1.000000000000000000) ) ) 
 REPRESENTATION_ITEM ( '' )  SURFACE ( )  );
#9514 = CIRCLE ( 'NONE', #7786, 2.500000000000000000 ) ;
#9515 = CIRCLE ( 'NONE', #12914, 0.6412116890856960350 ) ;
#9516 = CARTESIAN_POINT ( 'NONE',  ( 0.9749999999999999778, -0.4829448521957645513, -0.3750000000000000555 ) ) ;
#9517 = ORIENTED_EDGE ( 'NONE', *, *, #3238, .T. ) ;
#9518 = AXIS2_PLACEMENT_3D ( 'NONE', #11170, #1827, #2842 ) ;
#9519 = CARTESIAN_POINT ( 'NONE',  ( 3.441118530312176738, 1.974988295543748329, -0.6122333929865744206 ) ) ;
#9520 = LINE ( 'NONE', #8306, #14715 ) ;
#9521 = CARTESIAN_POINT ( 'NONE',  ( 3.875000000000000000, 3.085321731235734610, 0.5849999999999996314 ) ) ;
#9522 = AXIS2_PLACEMENT_3D ( 'NONE', #12814, #12507, #5565 ) ;
#9523 = LINE ( 'NONE', #9597, #12103 ) ;
#9524 = ORIENTED_EDGE ( 'NONE', *, *, #1372, .T. ) ;
#9525 = FACE_OUTER_BOUND ( 'NONE', #11211, .T. ) ;
#9526 = LINE ( 'NONE', #8077, #5223 ) ;
#9527 = ORIENTED_EDGE ( 'NONE', *, *, #9407, .F. ) ;
#9528 = ADVANCED_FACE ( 'NONE', ( #6583 ), #3434, .T. ) ;
#9529 = DIRECTION ( 'NONE',  ( -1.000000000000000000, -0.000000000000000000, -0.000000000000000000 ) ) ;
#9530 = EDGE_CURVE ( 'NONE', #392, #6113, #836, .T. ) ;
#9531 = ADVANCED_FACE ( 'NONE', ( #736 ), #15023, .F. ) ;
#9532 =( GEOMETRIC_REPRESENTATION_CONTEXT ( 3 ) GLOBAL_UNCERTAINTY_ASSIGNED_CONTEXT ( ( #2490 ) ) GLOBAL_UNIT_ASSIGNED_CONTEXT ( ( #14703, #1838, #8891 ) ) REPRESENTATION_CONTEXT ( 'NONE', 'WORKASPACE' ) );
#9533 = CARTESIAN_POINT ( 'NONE',  ( 0.06299999999999998657, 0.000000000000000000, 0.000000000000000000 ) ) ;
#9534 = CONICAL_SURFACE ( 'NONE', #8067, 0.4849999999999995981, 0.7853981633974598253 ) ;
#9535 = DIRECTION ( 'NONE',  ( 0.000000000000000000, -1.000000000000000000, 0.000000000000000000 ) ) ;
#9536 = EDGE_CURVE ( 'NONE', #9198, #9590, #11606, .T. ) ;
#9537 = CARTESIAN_POINT ( 'NONE',  ( 0.1164708448095412852, 0.000000000000000000, -0.9176380235743023528 ) ) ;
#9538 = VERTEX_POINT ( 'NONE', #12981 ) ;
#9539 = ORIENTED_EDGE ( 'NONE', *, *, #12713, .F. ) ;
#9540 = ORIENTED_EDGE ( 'NONE', *, *, #4853, .F. ) ;
#9541 = AXIS2_PLACEMENT_3D ( 'NONE', #5154, #14468, #13172 ) ;
#9542 = FACE_OUTER_BOUND ( 'NONE', #7691, .T. ) ;
#9543 =( BOUNDED_CURVE ( )  B_SPLINE_CURVE ( 3, ( #64, #7571, #1668, #6360 ),
 .UNSPECIFIED., .F., .F. ) 
 B_SPLINE_CURVE_WITH_KNOTS ( ( 4, 4 ),
 ( 4.712388980384689674, 5.497787143782139729 ),
 .UNSPECIFIED. ) 
 CURVE ( )  GEOMETRIC_REPRESENTATION_ITEM ( )  RATIONAL_B_SPLINE_CURVE ( ( 1.000000000000000000, 0.9492530216741910110, 0.9492530216741910110, 1.000000000000000000 ) ) 
 REPRESENTATION_ITEM ( '' )  );
#9544 = CARTESIAN_POINT ( 'NONE',  ( 3.394491571325183088, 1.679378605318059048, 1.941878605318041462 ) ) ;
#9545 = DIRECTION ( 'NONE',  ( 0.9396926207859107594, -0.000000000000000000, 0.3420201433256624401 ) ) ;
#9546 = DIRECTION ( 'NONE',  ( 1.000000000000000000, 0.000000000000000000, 0.000000000000000000 ) ) ;
#9547 = ORIENTED_EDGE ( 'NONE', *, *, #14654, .T. ) ;
#9548 = CARTESIAN_POINT ( 'NONE',  ( 0.6179999999999965521, 1.679378605318059492, 1.304378605318041062 ) ) ;
#9549 = CARTESIAN_POINT ( 'NONE',  ( 1.993930392107535754, 0.2778841324402123725, 0.4718371413544162341 ) ) ;
#9550 = CARTESIAN_POINT ( 'NONE',  ( -0.4125000000000001998, 0.1859999999999983611, -0.3725000000000000533 ) ) ;
#9551 = ADVANCED_FACE ( 'NONE', ( #8412 ), #6119, .T. ) ;
#9552 =( CONVERSION_BASED_UNIT ( 'INCH', #14121 ) LENGTH_UNIT ( ) NAMED_UNIT ( #388 ) );
#9553 = CARTESIAN_POINT ( 'NONE',  ( 4.420609161099084083, 1.729170253341261843, -0.5175182154212143448 ) ) ;
#9554 = VERTEX_POINT ( 'NONE', #10548 ) ;
#9556 = EDGE_LOOP ( 'NONE', ( #14798, #3952, #8832, #12246 ) ) ;
#9555 = CARTESIAN_POINT ( 'NONE',  ( 3.876560711617219379, 3.137999999999999901, 0.000000000000000000 ) ) ;
#9557 = EDGE_CURVE ( 'NONE', #4765, #4181, #9891, .T. ) ;
#9558 = EDGE_LOOP ( 'NONE', ( #13758, #712 ) ) ;
#9559 = LINE ( 'NONE', #6956, #618 ) ;
#9560 = ORIENTED_EDGE ( 'NONE', *, *, #12163, .T. ) ;
#9561 = CARTESIAN_POINT ( 'NONE',  ( 0.06299999999999994493, 1.679378605318059492, 1.272378605318035927 ) ) ;
#9562 = APPLICATION_PROTOCOL_DEFINITION ( 'draft international standard', 'automotive_design', 1998, #14363 ) ;
#9563 = FACE_OUTER_BOUND ( 'NONE', #7527, .T. ) ;
#9564 = VERTEX_POINT ( 'NONE', #3506 ) ;
#9565 = DIRECTION ( 'NONE',  ( 0.000000000000000000, 0.000000000000000000, -1.000000000000000000 ) ) ;
#9566 = DIRECTION ( 'NONE',  ( -0.5000000000000000000, 0.000000000000000000, 0.8660254037844385966 ) ) ;
#9567 = B_SPLINE_CURVE_WITH_KNOTS ( 'NONE', 3,
 ( #8435, #1526, #2537, #13002 ),
 .UNSPECIFIED., .F., .F.,
 ( 4, 4 ),
 ( 0.000000000000000000, 0.0001090996491984598624 ),
 .UNSPECIFIED. ) ;
#9568 = CARTESIAN_POINT ( 'NONE',  ( 3.834759817877919197, 1.869817227414270588, 0.7491158427897641747 ) ) ;
#9569 = FACE_OUTER_BOUND ( 'NONE', #7168, .T. ) ;
#9570 = AXIS2_PLACEMENT_3D ( 'NONE', #6793, #3339, #8016 ) ;
#9571 = CARTESIAN_POINT ( 'NONE',  ( 8.559253539154882517, 0.8718469098602882328, 0.3109429831200923311 ) ) ;
#9572 = CARTESIAN_POINT ( 'NONE',  ( 2.774999999999999911, -2.359999999999984333, 1.575000000000016387 ) ) ;
#9573 = CARTESIAN_POINT ( 'NONE',  ( 3.437600372662337200, 2.055609121798811501, 0.6090298485159663100 ) ) ;
#9574 = CARTESIAN_POINT ( 'NONE',  ( 4.647180688011975036, 1.726985733735235007, -0.2447955753616387065 ) ) ;
#9575 = EDGE_CURVE ( 'NONE', #2708, #2201, #10777, .T. ) ;
#9576 = EDGE_CURVE ( 'NONE', #8125, #2908, #1336, .T. ) ;
#9577 = VERTEX_POINT ( 'NONE', #265 ) ;
#9578 = DIRECTION ( 'NONE',  ( 0.000000000000000000, 0.000000000000000000, -1.000000000000000000 ) ) ;
#9580 = EDGE_LOOP ( 'NONE', ( #14518, #3069, #12868, #8771 ) ) ;
#9579 = DIRECTION ( 'NONE',  ( -0.000000000000000000, 1.000000000000000000, -0.000000000000000000 ) ) ;
#9581 = VERTEX_POINT ( 'NONE', #1427 ) ;
#9582 = CARTESIAN_POINT ( 'NONE',  ( 2.124999999999999556, -2.360000000000000320, 0.9799999999999999822 ) ) ;
#9583 = DIRECTION ( 'NONE',  ( -1.000000000000000000, -0.000000000000000000, -0.000000000000000000 ) ) ;
#9584 = CARTESIAN_POINT ( 'NONE',  ( 2.634365942216866152, 0.3629388174706738024, 0.4627914414941119436 ) ) ;
#9585 = ORIENTED_EDGE ( 'NONE', *, *, #12508, .F. ) ;
#9586 = PRESENTATION_LAYER_ASSIGNMENT (  '', '', ( #7373 ) ) ;
#9587 = CARTESIAN_POINT ( 'NONE',  ( 0.000000000000000000, 1.239999999999999991, 0.000000000000000000 ) ) ;
#9588 = CARTESIAN_POINT ( 'NONE',  ( 2.774999999999999911, -2.360000000000016751, -0.9799999999999431388 ) ) ;
#9589 = FACE_OUTER_BOUND ( 'NONE', #9556, .T. ) ;
#9590 = VERTEX_POINT ( 'NONE', #8188 ) ;
#9591 = CARTESIAN_POINT ( 'NONE',  ( 2.774999999999999911, -2.399999999999999911, 0.6999999999999997335 ) ) ;
#9592 = CARTESIAN_POINT ( 'NONE',  ( 0.3725000000000000533, 0.000000000000000000, 0.3724999999999999978 ) ) ;
#9593 = AXIS2_PLACEMENT_3D ( 'NONE', #12626, #2147, #6839 ) ;
#9594 = CARTESIAN_POINT ( 'NONE',  ( 3.426491571325181340, -0.9799999999999436939, 2.360000000000016307 ) ) ;
#9595 = DIRECTION ( 'NONE',  ( -1.000000000000000000, 0.000000000000000000, 0.000000000000000000 ) ) ;
#9596 = EDGE_LOOP ( 'NONE', ( #1399, #12496, #13930, #7059 ) ) ;
#9597 = CARTESIAN_POINT ( 'NONE',  ( 0.06299999999999994493, 0.000000000000000000, -2.967999999999998639 ) ) ;
#9598 = ADVANCED_FACE ( 'NONE', ( #7190, #192, #15137, #12829 ), #3742, .F. ) ;
#9599 = ORIENTED_EDGE ( 'NONE', *, *, #1373, .T. ) ;
#9600 = CARTESIAN_POINT ( 'NONE',  ( 3.426491571325181340, 0.000000000000000000, 0.000000000000000000 ) ) ;
#9601 = EDGE_LOOP ( 'NONE', ( #6938, #14650, #8606, #14084 ) ) ;
#9602 = CARTESIAN_POINT ( 'NONE',  ( 0.000000000000000000, 5.750000000000000000, 0.4108223460329293864 ) ) ;
#9603 = CARTESIAN_POINT ( 'NONE',  ( 6.215861650065340527, 0.000000000000000000, 0.000000000000000000 ) ) ;
#9604 = DIRECTION ( 'NONE',  ( -0.000000000000000000, -1.000000000000000000, -0.000000000000000000 ) ) ;
#9605 = DIRECTION ( 'NONE',  ( 0.000000000000000000, 0.000000000000000000, 1.000000000000000000 ) ) ;
#9606 = EDGE_CURVE ( 'NONE', #3169, #9554, #7122, .T. ) ;
#9607 = CIRCLE ( 'NONE', #7879, 0.4849999999999995981 ) ;
#9608 = EDGE_CURVE ( 'NONE', #498, #4318, #14285, .T. ) ;
#9609 = ORIENTED_EDGE ( 'NONE', *, *, #10072, .T. ) ;
#9610 = ORIENTED_EDGE ( 'NONE', *, *, #6617, .T. ) ;
#9611 = ORIENTED_EDGE ( 'NONE', *, *, #12964, .T. ) ;
#9612 = CARTESIAN_POINT ( 'NONE',  ( 1.014081760637643104, -0.4429513723158955973, -0.3902785865519532438 ) ) ;
#9613 = CARTESIAN_POINT ( 'NONE',  ( 0.1807106342563528367, 1.629999999999999893, 5.178337979384803075E-18 ) ) ;
#9614 = CARTESIAN_POINT ( 'NONE',  ( 3.080868217518119678, 0.9969999999999996643, 0.4564849121819474220 ) ) ;
#9615 = ADVANCED_FACE ( 'NONE', ( #5811, #11700, #14050, #11845, #8272, #4662 ), #13049, .F. ) ;
#9616 = DIRECTION ( 'NONE',  ( -1.000000000000000000, -0.000000000000000000, -0.000000000000000000 ) ) ;
#9617 = ORIENTED_EDGE ( 'NONE', *, *, #2286, .T. ) ;
#9618 = CARTESIAN_POINT ( 'NONE',  ( 3.538023853514577155, 1.962612250029136307, -0.3701161287706387637 ) ) ;
#9619 = DIRECTION ( 'NONE',  ( 0.000000000000000000, 0.000000000000000000, 1.000000000000000000 ) ) ;
#9620 = CARTESIAN_POINT ( 'NONE',  ( 3.426491571325181340, 0.000000000000000000, 0.000000000000000000 ) ) ;
#9621 = CARTESIAN_POINT ( 'NONE',  ( 2.774999999999999911, -1.679378605318059048, -1.679378605318041950 ) ) ;
#9622 = VECTOR ( 'NONE', #3092, 39.37007874015748143 ) ;
#9623 = ADVANCED_FACE ( 'NONE', ( #11775 ), #4968, .F. ) ;
#9624 = CIRCLE ( 'NONE', #1301, 0.2944999999999856066 ) ;
#9625 = EDGE_CURVE ( 'NONE', #2972, #15105, #6004, .T. ) ;
#9626 = ORIENTED_EDGE ( 'NONE', *, *, #3291, .T. ) ;
#9628 = ORIENTED_EDGE ( 'NONE', *, *, #1168, .F. ) ;
#9627 = CARTESIAN_POINT ( 'NONE',  ( 0.3724999999999999423, 0.2159999999999999420, 0.4425000000000003930 ) ) ;
#9629 = ORIENTED_EDGE ( 'NONE', *, *, #11142, .F. ) ;
#9630 = CARTESIAN_POINT ( 'NONE',  ( 0.7100000000000001865, 1.901497511147139923E-16, -1.552690549202460968 ) ) ;
#9631 = VERTEX_POINT ( 'NONE', #6037 ) ;
#9632 = DIRECTION ( 'NONE',  ( -0.03173230733822608035, 0.000000000000000000, 0.9994964035307943861 ) ) ;
#9633 = CARTESIAN_POINT ( 'NONE',  ( 3.426491571325181340, -0.9799999999999436939, 3.360000000000016751 ) ) ;
#9634 = EDGE_LOOP ( 'NONE', ( #9314, #6312 ) ) ;
#9635 = VECTOR ( 'NONE', #12918, 39.37007874015748143 ) ;
#9636 = CARTESIAN_POINT ( 'NONE',  ( 3.426491571325181340, 1.575000000000016387, 2.359999999999999432 ) ) ;
#9637 = DIRECTION ( 'NONE',  ( -1.000000000000000000, -0.000000000000000000, -0.000000000000000000 ) ) ;
#9638 = ADVANCED_FACE ( 'NONE', ( #4735 ), #1273, .T. ) ;
#9639 = CARTESIAN_POINT ( 'NONE',  ( 3.426491571325181340, 0.000000000000000000, 0.000000000000000000 ) ) ;
#9640 = ADVANCED_FACE ( 'NONE', ( #9563 ), #9485, .F. ) ;
#9641 = CARTESIAN_POINT ( 'NONE',  ( 6.208491571325183145, -1.679378605318047946, -1.304378605318053053 ) ) ;
#9642 = CARTESIAN_POINT ( 'NONE',  ( 0.8664489288624988017, -0.4696205524674798015, -0.4424002136836096000 ) ) ;
#9643 = CONICAL_SURFACE ( 'NONE', #1068, 0.3750000000000004996, 0.7853981633974621568 ) ;
#9644 = CARTESIAN_POINT ( 'NONE',  ( 3.638344611185302835, 1.884848995134380534, 0.7117177447420894865 ) ) ;
#9645 = DIRECTION ( 'NONE',  ( -0.000000000000000000, -1.000000000000000000, -0.000000000000000000 ) ) ;
#9646 = ORIENTED_EDGE ( 'NONE', *, *, #3237, .T. ) ;
#9647 = CARTESIAN_POINT ( 'NONE',  ( 0.6867356290494766036, -0.4821011294950960369, 0.4280493037418064417 ) ) ;
#9649 = VERTEX_POINT ( 'NONE', #10842 ) ;
#9648 = LINE ( 'NONE', #2296, #4061 ) ;
#9650 = EDGE_LOOP ( 'NONE', ( #12778, #2070, #7038, #1864, #1571, #1663, #5912, #2151, #464, #3708 ) ) ;
#9651 = LINE ( 'NONE', #8208, #5579 ) ;
#9652 = CARTESIAN_POINT ( 'NONE',  ( 3.249780665369845778, 0.6798122612590481451, 0.3942284963567643241 ) ) ;
#9653 = VERTEX_POINT ( 'NONE', #5180 ) ;
#9654 = CARTESIAN_POINT ( 'NONE',  ( 2.774999999999999911, -1.575000000000000178, 2.360000000000016751 ) ) ;
#9655 = CIRCLE ( 'NONE', #6466, 0.2945000000000006501 ) ;
#9656 = ADVANCED_FACE ( 'NONE', ( #7478 ), #3891, .T. ) ;
#9657 = ADVANCED_FACE ( 'NONE', ( #6186 ), #13057, .F. ) ;
#9658 = CARTESIAN_POINT ( 'NONE',  ( 0.6566194192392924567, -0.01184293933552419895, 0.4974488347804321142 ) ) ;
#9659 = DIRECTION ( 'NONE',  ( 1.000000000000000000, 0.000000000000000000, 0.000000000000000000 ) ) ;
#9660 = ORIENTED_EDGE ( 'NONE', *, *, #8134, .T. ) ;
#9661 = LINE ( 'NONE', #1601, #14119 ) ;
#9662 = DIRECTION ( 'NONE',  ( 1.000000000000000000, 0.000000000000000000, 0.000000000000000000 ) ) ;
#9663 = FACE_BOUND ( 'NONE', #13697, .T. ) ;
#9664 = ORIENTED_EDGE ( 'NONE', *, *, #10999, .T. ) ;
#9665 = AXIS2_PLACEMENT_3D ( 'NONE', #7946, #14981, #5505 ) ;
#9666 = DIRECTION ( 'NONE',  ( 1.874307916738608820E-16, -1.000000000000000000, -0.000000000000000000 ) ) ;
#9667 = EDGE_LOOP ( 'NONE', ( #14633, #3664, #9129, #3046 ) ) ;
#9668 = VECTOR ( 'NONE', #10346, 39.37007874015748143 ) ;
#9669 = CIRCLE ( 'NONE', #3547, 0.06000000000000001166 ) ;
#9670 = CARTESIAN_POINT ( 'NONE',  ( 2.124999999999999556, -0.9799999999999986500, -3.359999999999999876 ) ) ;
#9671 = ORIENTED_EDGE ( 'NONE', *, *, #2250, .T. ) ;
#9672 = CYLINDRICAL_SURFACE ( 'NONE', #13883, 0.4999999999999997224 ) ;
#9673 = CARTESIAN_POINT ( 'NONE',  ( 6.826491571325181695, 1.679378605318059492, 1.679378605318041506 ) ) ;
#9674 = ADVANCED_FACE ( 'NONE', ( #13200 ), #5749, .F. ) ;
#9675 = AXIS2_PLACEMENT_3D ( 'NONE', #3625, #8311, #8657 ) ;
#9676 = LINE ( 'NONE', #2559, #12645 ) ;
#9677 = CARTESIAN_POINT ( 'NONE',  ( 2.229630226914017577, 0.4287871555018993863, -0.4085020630706684974 ) ) ;
#9678 = CIRCLE ( 'NONE', #4288, 1.000000000000000222 ) ;
#9679 = CONICAL_SURFACE ( 'NONE', #2328, 1.000000000000000000, 0.7853981633974477239 ) ;
#9680 = DIRECTION ( 'NONE',  ( 0.000000000000000000, 0.000000000000000000, 1.000000000000000000 ) ) ;
#9681 = VERTEX_POINT ( 'NONE', #2881 ) ;
#9682 = VERTEX_POINT ( 'NONE', #410 ) ;
#9683 = VERTEX_POINT ( 'NONE', #14430 ) ;
#9684 = VECTOR ( 'NONE', #8592, 39.37007874015748143 ) ;
#9685 = CARTESIAN_POINT ( 'NONE',  ( 8.665761398406338856, 0.8755662462622739728, -0.3295708899403233527 ) ) ;
#9686 = CARTESIAN_POINT ( 'NONE',  ( 0.2099999999999999922, 0.7512260236060024354, 0.3809527529760087239 ) ) ;
#9687 = AXIS2_PLACEMENT_3D ( 'NONE', #427, #2529, #3970 ) ;
#9688 = DIRECTION ( 'NONE',  ( 0.7071067811865376918, 8.659560562355053653E-17, 0.7071067811865573427 ) ) ;
#9689 = CYLINDRICAL_SURFACE ( 'NONE', #8523, 0.3750000000000007772 ) ;
#9690 = DIRECTION ( 'NONE',  ( 0.000000000000000000, -1.000000000000000000, 0.000000000000000000 ) ) ;
#9691 = LENGTH_MEASURE_WITH_UNIT ( LENGTH_MEASURE( 0.02539999999999999897 ), #10048 );
#9692 = VECTOR ( 'NONE', #3909, 39.37007874015748143 ) ;
#9693 = DIRECTION ( 'NONE',  ( 1.000000000000000000, 0.000000000000000000, 0.000000000000000000 ) ) ;
#9694 = ORIENTED_EDGE ( 'NONE', *, *, #7838, .F. ) ;
#9695 = ORIENTED_EDGE ( 'NONE', *, *, #2452, .T. ) ;
#9696 = EDGE_LOOP ( 'NONE', ( #961, #5656, #13008, #12225 ) ) ;
#9697 = CARTESIAN_POINT ( 'NONE',  ( -0.4349147617188414694, 1.239999999999999991, -0.008611041693271251005 ) ) ;
#9698 = CARTESIAN_POINT ( 'NONE',  ( 0.000000000000000000, 0.000000000000000000, 0.000000000000000000 ) ) ;
#9699 = CARTESIAN_POINT ( 'NONE',  ( 4.358375425022244620, 0.9917754135670810989, 0.1321374421498176799 ) ) ;
#9700 = CIRCLE ( 'NONE', #3104, 0.8499999999999999778 ) ;
#9701 =( LENGTH_UNIT ( ) NAMED_UNIT ( * ) SI_UNIT ( $, .METRE. ) );
#9702 = DIRECTION ( 'NONE',  ( 0.000000000000000000, 0.000000000000000000, 1.000000000000000000 ) ) ;
#9703 = ORIENTED_EDGE ( 'NONE', *, *, #4214, .T. ) ;
#9704 = CARTESIAN_POINT ( 'NONE',  ( 6.176491571325181340, 1.679378605318059492, 1.679378605318041506 ) ) ;
#9705 = CARTESIAN_POINT ( 'NONE',  ( 2.774999999999999911, -1.575000000000027489, -2.359999999999989218 ) ) ;
#9706 = EDGE_CURVE ( 'NONE', #2309, #13167, #12331, .T. ) ;
#9707 = EDGE_CURVE ( 'NONE', #159, #12504, #5328, .T. ) ;
#9708 = LINE ( 'NONE', #14358, #11457 ) ;
#9709 = ADVANCED_FACE ( 'NONE', ( #13424 ), #3959, .F. ) ;
#9710 = AXIS2_PLACEMENT_3D ( 'NONE', #190, #14204, #13047 ) ;
#9711 = PRODUCT_DEFINITION_SHAPE ( 'NONE', 'NONE',  #15164 ) ;
#9712 = FACE_BOUND ( 'NONE', #7191, .T. ) ;
#9713 = CARTESIAN_POINT ( 'NONE',  ( 4.769268701363833074, 3.567999999999999616, -0.3249191361593797289 ) ) ;
#9714 = EDGE_CURVE ( 'NONE', #251, #13167, #7550, .T. ) ;
#9715 = CIRCLE ( 'NONE', #3115, 2.000179419058113695 ) ;
#9716 = CARTESIAN_POINT ( 'NONE',  ( 3.720984570872676755, 1.852166139790340837, 0.7347827700683455809 ) ) ;
#9717 = CARTESIAN_POINT ( 'NONE',  ( 4.344846310392954436, 3.567999999999999616, -1.491010071662831171 ) ) ;
#9718 = ORIENTED_EDGE ( 'NONE', *, *, #9576, .T. ) ;
#9719 = CARTESIAN_POINT ( 'NONE',  ( 6.096491571325181269, 0.000000000000000000, 0.000000000000000000 ) ) ;
#9721 = ORIENTED_EDGE ( 'NONE', *, *, #10289, .T. ) ;
#9720 = DIRECTION ( 'NONE',  ( 1.000000000000000000, 0.000000000000000000, 0.000000000000000000 ) ) ;
#9722 = ORIENTED_EDGE ( 'NONE', *, *, #6080, .F. ) ;
#9723 = CONICAL_SURFACE ( 'NONE', #5083, 0.4070000000000022489, 0.7853981633974547183 ) ;
#9724 = CARTESIAN_POINT ( 'NONE',  ( 0.6552635435737792502, -0.03280443401857551650, 0.5075266421723674259 ) ) ;
#9725 = DIRECTION ( 'NONE',  ( 0.000000000000000000, 0.000000000000000000, -1.000000000000000000 ) ) ;
#9726 = ORIENTED_EDGE ( 'NONE', *, *, #5881, .F. ) ;
#9727 = LINE ( 'NONE', #12937, #7305 ) ;
#9728 = AXIS2_PLACEMENT_3D ( 'NONE', #3477, #5701, #4326 ) ;
#9729 = CARTESIAN_POINT ( 'NONE',  ( 2.774999999999999911, -1.575000000000000178, 2.360000000000016751 ) ) ;
#9730 = DIRECTION ( 'NONE',  ( 0.4999999999999998335, 0.000000000000000000, 0.8660254037844388186 ) ) ;
#9731 = ORIENTED_EDGE ( 'NONE', *, *, #9207, .T. ) ;
#9732 = CARTESIAN_POINT ( 'NONE',  ( 2.124999999999999556, 0.000000000000000000, 0.000000000000000000 ) ) ;
#9733 = DIRECTION ( 'NONE',  ( 0.000000000000000000, 1.000000000000000000, 0.000000000000000000 ) ) ;
#9734 = LINE ( 'NONE', #12023, #11941 ) ;
#9735 = EDGE_CURVE ( 'NONE', #8646, #6726, #14360, .T. ) ;
#9736 = AXIS2_PLACEMENT_3D ( 'NONE', #13724, #12660, #1955 ) ;
#9737 = FACE_OUTER_BOUND ( 'NONE', #11503, .T. ) ;
#9738 = ORIENTED_EDGE ( 'NONE', *, *, #12482, .F. ) ;
#9739 = ADVANCED_FACE ( 'NONE', ( #1501 ), #2669, .T. ) ;
#9740 = CARTESIAN_POINT ( 'NONE',  ( -0.4021230921906706057, 1.589827634136291135, 0.06540787938107404942 ) ) ;
#9741 = ORIENTED_EDGE ( 'NONE', *, *, #6288, .F. ) ;
#9742 = SURFACE_STYLE_FILL_AREA ( #8251 ) ;
#9743 = AXIS2_PLACEMENT_3D ( 'NONE', #12707, #2233, #12939 ) ;
#9744 = CARTESIAN_POINT ( 'NONE',  ( 0.7435009325572420336, -0.6334543218446812007, 0.000000000000000000 ) ) ;
#9745 = VECTOR ( 'NONE', #9782, 39.37007874015748143 ) ;
#9746 = CARTESIAN_POINT ( 'NONE',  ( 0.8364764264237143365, -0.4366331065633826669, -0.3349451187573404543 ) ) ;
#9747 = CIRCLE ( 'NONE', #11454, 0.3203340137431719414 ) ;
#9748 = CYLINDRICAL_SURFACE ( 'NONE', #8756, 0.3190000000000000058 ) ;
#9749 = AXIS2_PLACEMENT_3D ( 'NONE', #3211, #3438, #7949 ) ;
#9750 = VECTOR ( 'NONE', #12217, 39.37007874015748143 ) ;
#9751 = DIRECTION ( 'NONE',  ( -1.000000000000000000, -0.000000000000000000, -0.000000000000000000 ) ) ;
#9752 = VECTOR ( 'NONE', #11629, 39.37007874015748143 ) ;
#9753 = EDGE_LOOP ( 'NONE', ( #12167, #10506 ) ) ;
#9754 = VERTEX_POINT ( 'NONE', #13656 ) ;
#9755 = VERTEX_POINT ( 'NONE', #13572 ) ;
#9756 = EDGE_CURVE ( 'NONE', #8780, #2036, #10153, .T. ) ;
#9757 = CARTESIAN_POINT ( 'NONE',  ( 8.850000000000575184, 0.8820000000023066056, -0.04908333765187990194 ) ) ;
#9758 = MECHANICAL_DESIGN_GEOMETRIC_PRESENTATION_REPRESENTATION (  '', ( #15123 ), #12685 ) ;
#9759 = CARTESIAN_POINT ( 'NONE',  ( 2.124999999999999556, -1.575000000000000178, 2.360000000000016751 ) ) ;
#9760 = DIRECTION ( 'NONE',  ( 0.01412288512831213171, -3.675428035873182550E-19, -0.9999002670844991947 ) ) ;
#9761 = CARTESIAN_POINT ( 'NONE',  ( -0.4108223460329322729, 0.000000000000000000, 0.2849999999999953681 ) ) ;
#9762 = DIRECTION ( 'NONE',  ( 0.000000000000000000, 1.000000000000000000, 0.000000000000000000 ) ) ;
#9763 = CARTESIAN_POINT ( 'NONE',  ( 4.269212872948124904, 1.781133266760655864, -0.6394758128702182631 ) ) ;
#9764 = TOROIDAL_SURFACE ( 'NONE', #9541, 1.580000000000000071, 0.08000000000000000167 ) ;
#9765 = CARTESIAN_POINT ( 'NONE',  ( 4.338845464883685388, 1.779384211668088911, -0.5916759243745035590 ) ) ;
#9766 = ORIENTED_EDGE ( 'NONE', *, *, #9222, .T. ) ;
#9767 = ORIENTED_EDGE ( 'NONE', *, *, #4590, .F. ) ;
#9768 = ORIENTED_EDGE ( 'NONE', *, *, #5955, .T. ) ;
#9769 = CARTESIAN_POINT ( 'NONE',  ( 3.874999999999999556, 2.750000000000000000, 1.320000000000000062 ) ) ;
#9770 = EDGE_CURVE ( 'NONE', #6864, #12484, #14618, .T. ) ;
#9771 = DIRECTION ( 'NONE',  ( 0.000000000000000000, -1.000000000000000000, -0.000000000000000000 ) ) ;
#9772 = CARTESIAN_POINT ( 'NONE',  ( 4.037927003766942136, 0.8807194764073917881, 0.4738554624952319161 ) ) ;
#9773 = PRODUCT_CONTEXT ( 'NONE', #8616, 'mechanical' ) ;
#9774 = CARTESIAN_POINT ( 'NONE',  ( 3.874999999999999556, 3.137999999999999901, 1.320000000000000062 ) ) ;
#9775 = ORIENTED_EDGE ( 'NONE', *, *, #4094, .F. ) ;
#9776 = DIRECTION ( 'NONE',  ( -1.000000000000000000, -0.000000000000000000, -0.000000000000000000 ) ) ;
#9777 = DIRECTION ( 'NONE',  ( -0.000000000000000000, -1.000000000000000000, -0.000000000000000000 ) ) ;
#9778 = CIRCLE ( 'NONE', #12452, 0.1899999999999996136 ) ;
#9779 = CARTESIAN_POINT ( 'NONE',  ( 3.599442323206996530, 1.969410324051942274, 0.6972124116338633826 ) ) ;
#9780 = CYLINDRICAL_SURFACE ( 'NONE', #10658, 0.03999999999999998002 ) ;
#9781 = DIRECTION ( 'NONE',  ( -0.000000000000000000, -1.000000000000000000, 0.000000000000000000 ) ) ;
#9782 = DIRECTION ( 'NONE',  ( 8.659560562354973534E-17, 0.7071067811865441310, -0.7071067811865509034 ) ) ;
#9783 = CARTESIAN_POINT ( 'NONE',  ( 3.825335190572127786, 1.816349960665768037, 0.7486281390988553941 ) ) ;
#9784 = EDGE_CURVE ( 'NONE', #13032, #2839, #8598, .T. ) ;
#9785 = DIRECTION ( 'NONE',  ( 8.659560562354890950E-17, 0.7071067811865509034, -0.7071067811865441310 ) ) ;
#9786 = EDGE_CURVE ( 'NONE', #3470, #14655, #11316, .T. ) ;
#9787 = ORIENTED_EDGE ( 'NONE', *, *, #7093, .F. ) ;
#9788 = ADVANCED_FACE ( 'NONE', ( #12502 ), #4866, .F. ) ;
#9789 = DIRECTION ( 'NONE',  ( 0.000000000000000000, -1.000000000000000000, 0.000000000000000000 ) ) ;
#9791 = VERTEX_POINT ( 'NONE', #6636 ) ;
#9790 = CARTESIAN_POINT ( 'NONE',  ( 5.567023771132172172, 0.000000000000000000, 0.000000000000000000 ) ) ;
#9792 = ORIENTED_EDGE ( 'NONE', *, *, #5280, .T. ) ;
#9793 = CARTESIAN_POINT ( 'NONE',  ( 0.6609607771814278721, 0.006241162926370197317, 0.4835552281312084921 ) ) ;
#9794 = LINE ( 'NONE', #9946, #14531 ) ;
#9795 = ORIENTED_EDGE ( 'NONE', *, *, #12305, .T. ) ;
#9796 = CARTESIAN_POINT ( 'NONE',  ( -0.09035531712817639061, 1.379999999999999671, 0.1565000000000000280 ) ) ;
#9797 = CARTESIAN_POINT ( 'NONE',  ( 2.806999999999999940, -1.679378605318059048, -1.416878605318056872 ) ) ;
#9798 = ADVANCED_FACE ( 'NONE', ( #11524 ), #4339, .F. ) ;
#9799 = AXIS2_PLACEMENT_3D ( 'NONE', #5720, #2430, #9473 ) ;
#9800 = CARTESIAN_POINT ( 'NONE',  ( 0.7058998964907849949, -0.06000000000000026840, 0.4900296624789436950 ) ) ;
#9801 = LINE ( 'NONE', #3920, #2653 ) ;
#9802 = ORIENTED_EDGE ( 'NONE', *, *, #8858, .T. ) ;
#9803 = CARTESIAN_POINT ( 'NONE',  ( 2.034917172172060251, -0.2365099525741251041, -0.4116907716851759269 ) ) ;
#9804 = CARTESIAN_POINT ( 'NONE',  ( 2.980731298636167370, 2.750000000000000000, -0.3249191361593797844 ) ) ;
#9805 = EDGE_CURVE ( 'NONE', #184, #14657, #13624, .T. ) ;
#9806 = DIRECTION ( 'NONE',  ( -1.000000000000000000, -0.000000000000000000, -0.000000000000000000 ) ) ;
#9807 = MECHANICAL_DESIGN_GEOMETRIC_PRESENTATION_REPRESENTATION (  '', ( #7373 ), #6893 ) ;
#9808 = CARTESIAN_POINT ( 'NONE',  ( 0.6179999999999965521, 1.679378605318059492, 1.679378605318041506 ) ) ;
#9809 = VERTEX_POINT ( 'NONE', #1023 ) ;
#9810 = CARTESIAN_POINT ( 'NONE',  ( -0.3932619838309059368, 1.593633255602467713, 0.08075576927155943274 ) ) ;
#9811 = ORIENTED_EDGE ( 'NONE', *, *, #7569, .F. ) ;
#9812 = CARTESIAN_POINT ( 'NONE',  ( 2.230477600021715467, 0.4287871555018996084, 0.4684960790957384824 ) ) ;
#9813 = DIRECTION ( 'NONE',  ( -1.000000000000000000, -0.000000000000000000, -0.000000000000000000 ) ) ;
#9814 = ADVANCED_FACE ( 'NONE', ( #3260 ), #2187, .T. ) ;
#9815 = CARTESIAN_POINT ( 'NONE',  ( 1.127821516536285484, -0.3829999999995594151, 0.4840703175630468036 ) ) ;
#9816 = CARTESIAN_POINT ( 'NONE',  ( 0.7809470991741572776, -0.4447677964980547571, -0.3372808541555822881 ) ) ;
#9817 = CONICAL_SURFACE ( 'NONE', #3220, 0.2625000000000000111, 0.7853981633974621568 ) ;
#9818 = CARTESIAN_POINT ( 'NONE',  ( 0.06299999999999994493, 0.000000000000000000, -2.967999999999998639 ) ) ;
#9819 = ADVANCED_FACE ( 'NONE', ( #6870 ), #10376, .F. ) ;
#9820 = CARTESIAN_POINT ( 'NONE',  ( -0.1807106342563527812, 1.629999999999999893, 3.262375646219079751E-17 ) ) ;
#9821 =( NAMED_UNIT ( * ) SI_UNIT ( $, .STERADIAN. ) SOLID_ANGLE_UNIT ( ) );
#9822 = VERTEX_POINT ( 'NONE', #5413 ) ;
#9823 = ORIENTED_EDGE ( 'NONE', *, *, #8038, .F. ) ;
#9824 = ORIENTED_EDGE ( 'NONE', *, *, #12144, .T. ) ;
#9825 = DIRECTION ( 'NONE',  ( 0.000000000000000000, -1.000000000000000000, 0.000000000000000000 ) ) ;
#9826 = CARTESIAN_POINT ( 'NONE',  ( 3.426491571325181340, 1.224646799147353207E-16, -1.000000000000000000 ) ) ;
#9827 = DIRECTION ( 'NONE',  ( 0.000000000000000000, 0.000000000000000000, 1.000000000000000000 ) ) ;
#9828 = PRODUCT ( 'Lock Lever', 'Lock Lever', '', ( #12139 ) ) ;
#9829 = CARTESIAN_POINT ( 'NONE',  ( 8.695322983473955603, 0.9353919960747727469, -0.3771847036232491845 ) ) ;
#9830 = CARTESIAN_POINT ( 'NONE',  ( 4.134953843058370104, 1.794421708884817113, 0.7041910065148488940 ) ) ;
#9831 = AXIS2_PLACEMENT_3D ( 'NONE', #2392, #9293, #5761 ) ;
#9832 = EDGE_CURVE ( 'NONE', #10219, #1686, #10077, .T. ) ;
#9833 = EDGE_CURVE ( 'NONE', #6905, #5216, #7302, .T. ) ;
#9834 = CARTESIAN_POINT ( 'NONE',  ( 4.393220956986357173, 1.780595993968445034, -0.5448392271506915518 ) ) ;
#9835 = ORIENTED_EDGE ( 'NONE', *, *, #3683, .T. ) ;
#9836 = ORIENTED_EDGE ( 'NONE', *, *, #2502, .T. ) ;
#9837 = ORIENTED_EDGE ( 'NONE', *, *, #4120, .T. ) ;
#9838 = DIRECTION ( 'NONE',  ( 1.000000000000000000, 0.000000000000000000, 0.000000000000000000 ) ) ;
#9839 = AXIS2_PLACEMENT_3D ( 'NONE', #13315, #534, #1994 ) ;
#9840 = DIRECTION ( 'NONE',  ( -1.000000000000000000, -0.000000000000000000, -0.000000000000000000 ) ) ;
#9841 = CARTESIAN_POINT ( 'NONE',  ( 4.127139180425047904, 0.9016242830556325805, 0.4329707884123231154 ) ) ;
#9842 = CONTEXT_DEPENDENT_SHAPE_REPRESENTATION ( #10466, #12146 ) ;
#9843 = CARTESIAN_POINT ( 'NONE',  ( 3.874999999999999556, 3.535499999999999421, -1.320000000000000062 ) ) ;
#9844 = ORIENTED_EDGE ( 'NONE', *, *, #8797, .T. ) ;
#9845 = DIRECTION ( 'NONE',  ( -1.000000000000000000, -0.000000000000000000, -0.000000000000000000 ) ) ;
#9846 = DIRECTION ( 'NONE',  ( 0.000000000000000000, 0.000000000000000000, 1.000000000000000000 ) ) ;
#9847 = DIRECTION ( 'NONE',  ( -1.000000000000000000, -0.000000000000000000, -0.000000000000000000 ) ) ;
#9848 = AXIS2_PLACEMENT_3D ( 'NONE', #8024, #2352, #109 ) ;
#9849 = EDGE_CURVE ( 'NONE', #1866, #8413, #12578, .T. ) ;
#9850 = DIRECTION ( 'NONE',  ( -0.9396926207859105373, 0.000000000000000000, -0.3420201433256627732 ) ) ;
#9851 = LINE ( 'NONE', #11376, #1527 ) ;
#9852 = DIRECTION ( 'NONE',  ( 1.000000000000000000, 0.000000000000000000, -3.779312718515659280E-16 ) ) ;
#9853 = LINE ( 'NONE', #14507, #6325 ) ;
#9854 = VECTOR ( 'NONE', #3520, 39.37007874015748143 ) ;
#9856 = EDGE_LOOP ( 'NONE', ( #5922, #629, #11525, #3277, #1321, #7809, #11099, #12271, #6385, #14136, #6198, #12846, #5657, #1177, #11846, #2164, #5952, #13147, #9055, #12371, #66, #405, #7496, #3545, #8575 ) ) ;
#9855 = DIRECTION ( 'NONE',  ( -1.000000000000000000, -0.000000000000000000, -0.000000000000000000 ) ) ;
#9857 = ORIENTED_EDGE ( 'NONE', *, *, #13660, .F. ) ;
#9858 = AXIS2_PLACEMENT_3D ( 'NONE', #3440, #6894, #11710 ) ;
#9859 = CARTESIAN_POINT ( 'NONE',  ( 2.186775859711120873, 0.4707856020413885290, 0.4085081077081219592 ) ) ;
#9861 = EDGE_LOOP ( 'NONE', ( #14560, #9503, #965, #6662 ) ) ;
#9860 = DIRECTION ( 'NONE',  ( -0.000000000000000000, -1.000000000000000000, -0.000000000000000000 ) ) ;
#9862 = EDGE_LOOP ( 'NONE', ( #1932, #12156, #828, #2254, #10206, #6333, #1996, #5392, #7185 ) ) ;
#9863 = AXIS2_PLACEMENT_3D ( 'NONE', #12867, #10585, #3397 ) ;
#9864 = FACE_OUTER_BOUND ( 'NONE', #12299, .T. ) ;
#9865 = DIRECTION ( 'NONE',  ( 0.000000000000000000, 0.000000000000000000, -1.000000000000000000 ) ) ;
#9866 = VERTEX_POINT ( 'NONE', #3724 ) ;
#9867 = CARTESIAN_POINT ( 'NONE',  ( -0.2099999999999999922, 1.239999999999999991, -0.3809527529760087239 ) ) ;
#9868 = CARTESIAN_POINT ( 'NONE',  ( 1.003158059735369090, -0.4829975555521401898, -0.4258273028168328422 ) ) ;
#9869 = DIRECTION ( 'NONE',  ( 0.000000000000000000, 1.000000000000000000, 0.000000000000000000 ) ) ;
#9870 = ADVANCED_FACE ( 'NONE', ( #10603 ), #9391, .T. ) ;
#9871 = B_SPLINE_CURVE_WITH_KNOTS ( 'NONE', 3,
 ( #14574, #10990, #10771, #5177, #1423, #12059, #9920, #8775, #6182, #3955, #4103, #480, #7404, #8621 ),
 .UNSPECIFIED., .F., .F.,
 ( 4, 2, 2, 2, 2, 2, 4 ),
 ( 0.02339532894303460175, 0.02409265248687545574, 0.02478997603071630973, 0.02618462311839802464, 0.02757927020607973956, 0.02827659374992059355, 0.02897391729376145100 ),
 .UNSPECIFIED. ) ;
#9872 = CARTESIAN_POINT ( 'NONE',  ( 0.6757896753473211504, -0.06125439598094604282, 0.4909021876970666720 ) ) ;
#9873 = AXIS2_PLACEMENT_3D ( 'NONE', #3967, #2895, #1658 ) ;
#9874 =( GEOMETRIC_REPRESENTATION_CONTEXT ( 3 ) GLOBAL_UNCERTAINTY_ASSIGNED_CONTEXT ( ( #1248 ) ) GLOBAL_UNIT_ASSIGNED_CONTEXT ( ( #2906, #7720, #6426 ) ) REPRESENTATION_CONTEXT ( 'NONE', 'WORKASPACE' ) );
#9875 = ORIENTED_EDGE ( 'NONE', *, *, #1577, .T. ) ;
#9876 = CARTESIAN_POINT ( 'NONE',  ( 2.775039370078740131, 1.679378605318059492, 2.054378605318042172 ) ) ;
#9877 = CARTESIAN_POINT ( 'NONE',  ( 0.6500000000000001332, -1.679378605318047946, -1.272378605318049027 ) ) ;
#9878 = FILL_AREA_STYLE ('',( #3987 ) ) ;
#9879 = ORIENTED_EDGE ( 'NONE', *, *, #8965, .F. ) ;
#9880 = CARTESIAN_POINT ( 'NONE',  ( 4.298848810396105335, 0.9641482059274013583, -0.2657306241200046992 ) ) ;
#9881 = DIRECTION ( 'NONE',  ( 0.000000000000000000, 0.000000000000000000, -1.000000000000000000 ) ) ;
#9882 = ORIENTED_EDGE ( 'NONE', *, *, #13877, .T. ) ;
#9883 = AXIS2_PLACEMENT_3D ( 'NONE', #10645, #3321, #4838 ) ;
#9884 = DIRECTION ( 'NONE',  ( -1.000000000000000000, 0.000000000000000000, 0.000000000000000000 ) ) ;
#9885 = VERTEX_POINT ( 'NONE', #1103 ) ;
#9886 = CARTESIAN_POINT ( 'NONE',  ( 3.874999999999999556, 3.535499999999999421, -1.130000000000000560 ) ) ;
#9887 = EDGE_CURVE ( 'NONE', #261, #13454, #4797, .T. ) ;
#9888 = CARTESIAN_POINT ( 'NONE',  ( 0.8386818780009405172, -0.4394694382868568061, -0.3315263062002954952 ) ) ;
#9889 = EDGE_CURVE ( 'NONE', #7304, #13246, #14112, .T. ) ;
#9890 = DIRECTION ( 'NONE',  ( -1.000000000000000000, -0.000000000000000000, -0.000000000000000000 ) ) ;
#9891 = CIRCLE ( 'NONE', #8920, 1.124999999999998446 ) ;
#9892 = DIRECTION ( 'NONE',  ( 0.000000000000000000, 1.000000000000000000, 0.000000000000000000 ) ) ;
#9893 = CIRCLE ( 'NONE', #3059, 0.2944999999999976525 ) ;
#9894 = CIRCLE ( 'NONE', #9169, 0.1899999999999996136 ) ;
#9895 = EDGE_CURVE ( 'NONE', #11537, #6001, #2407, .T. ) ;
#9896 =( BOUNDED_CURVE ( )  B_SPLINE_CURVE ( 3, ( #14447, #8800, #3975, #7642 ),
 .UNSPECIFIED., .F., .F. ) 
 B_SPLINE_CURVE_WITH_KNOTS ( ( 4, 4 ),
 ( 4.726512335037235779, 6.283185307179586232 ),
 .UNSPECIFIED. ) 
 CURVE ( )  GEOMETRIC_REPRESENTATION_ITEM ( )  RATIONAL_B_SPLINE_CURVE ( ( 1.000000000000000000, 0.8080549792898084061, 0.8080549792898084061, 1.000000000000000000 ) ) 
 REPRESENTATION_ITEM ( '' )  );
#9897 = DIRECTION ( 'NONE',  ( 0.000000000000000000, 0.000000000000000000, 1.000000000000000000 ) ) ;
#9898 = VERTEX_POINT ( 'NONE', #3572 ) ;
#9899 = ORIENTED_EDGE ( 'NONE', *, *, #6538, .F. ) ;
#9900 = ORIENTED_EDGE ( 'NONE', *, *, #12708, .T. ) ;
#9901 = EDGE_CURVE ( 'NONE', #5441, #9941, #13031, .T. ) ;
#9902 = CARTESIAN_POINT ( 'NONE',  ( 8.664307099992953454, 0.9344797629247183490, -0.3304588241376550384 ) ) ;
#9903 = ORIENTED_EDGE ( 'NONE', *, *, #3902, .F. ) ;
#9904 = DIRECTION ( 'NONE',  ( 0.000000000000000000, 0.000000000000000000, 1.000000000000000000 ) ) ;
#9905 = FACE_OUTER_BOUND ( 'NONE', #997, .T. ) ;
#9906 = CIRCLE ( 'NONE', #12834, 0.5174999999999995159 ) ;
#9907 = DIRECTION ( 'NONE',  ( 1.000000000000000000, 0.000000000000000000, 0.000000000000000000 ) ) ;
#9908 = AXIS2_PLACEMENT_3D ( 'NONE', #2323, #1082, #13938 ) ;
#9909 = CONICAL_SURFACE ( 'NONE', #3314, 1.932031071636253650, 0.2617993877991429685 ) ;
#9910 = CARTESIAN_POINT ( 'NONE',  ( 0.09035531712817647387, 1.629999999999999893, 0.1564999999999999447 ) ) ;
#9911 = EDGE_CURVE ( 'NONE', #6629, #6179, #1165, .T. ) ;
#9912 = VECTOR ( 'NONE', #6764, 39.37007874015748143 ) ;
#9913 = CARTESIAN_POINT ( 'NONE',  ( 4.124243424167258532, 1.725694442234845916, -0.7553927200278419685 ) ) ;
#9914 = EDGE_LOOP ( 'NONE', ( #5522, #1420 ) ) ;
#9915 = AXIS2_PLACEMENT_3D ( 'NONE', #3444, #6896, #9268 ) ;
#9916 = ORIENTED_EDGE ( 'NONE', *, *, #14463, .T. ) ;
#9917 = EDGE_CURVE ( 'NONE', #11151, #10316, #14122, .T. ) ;
#9918 = VECTOR ( 'NONE', #6200, 39.37007874015748854 ) ;
#9919 = ORIENTED_EDGE ( 'NONE', *, *, #8906, .T. ) ;
#9920 = CARTESIAN_POINT ( 'NONE',  ( 0.1264631971972072777, 1.593677921218988880, 0.3809527529760087794 ) ) ;
#9921 = CARTESIAN_POINT ( 'NONE',  ( 2.088768908813758873, 0.2870784642939425146, -0.4704976142822915319 ) ) ;
#9922 = CARTESIAN_POINT ( 'NONE',  ( 4.348661478442751083, 0.9870318323618022527, 0.1634103574579118534 ) ) ;
#9923 = EDGE_CURVE ( 'NONE', #7368, #5558, #10529, .T. ) ;
#9924 = CONTEXT_DEPENDENT_SHAPE_REPRESENTATION ( #10961, #5317 ) ;
#9925 = DIRECTION ( 'NONE',  ( -0.000000000000000000, 1.000000000000000000, -0.000000000000000000 ) ) ;
#9926 = VERTEX_POINT ( 'NONE', #6101 ) ;
#9927 = FACE_OUTER_BOUND ( 'NONE', #10653, .T. ) ;
#9928 = LINE ( 'NONE', #489, #2422 ) ;
#9929 = AXIS2_PLACEMENT_3D ( 'NONE', #10192, #4448, #8054 ) ;
#9930 = SHAPE_REPRESENTATION ( 'Inlet Housing', ( #8424 ), #9397 ) ;
#9931 = CARTESIAN_POINT ( 'NONE',  ( 0.7513246802501660770, -0.5029999999999998916, 0.4293820849162031661 ) ) ;
#9932 = DIRECTION ( 'NONE',  ( 0.000000000000000000, 0.000000000000000000, 1.000000000000000000 ) ) ;
#9933 = DIRECTION ( 'NONE',  ( 0.000000000000000000, 0.000000000000000000, -1.000000000000000000 ) ) ;
#9934 = CARTESIAN_POINT ( 'NONE',  ( 4.332693437952970683, 1.707681683440760656, 0.6520824339025526051 ) ) ;
#9936 = ORIENTED_EDGE ( 'NONE', *, *, #14541, .F. ) ;
#9935 = LINE ( 'NONE', #4122, #4017 ) ;
#9937 = CIRCLE ( 'NONE', #12126, 0.4849999999999995981 ) ;
#9938 = ORIENTED_EDGE ( 'NONE', *, *, #88, .T. ) ;
#9939 = CARTESIAN_POINT ( 'NONE',  ( -0.2405080627748324984, 1.577645543303435760, -0.3453333215960435187 ) ) ;
#9941 = VERTEX_POINT ( 'NONE', #7250 ) ;
#9940 = LINE ( 'NONE', #7494, #9190 ) ;
#9942 = ORIENTED_EDGE ( 'NONE', *, *, #10825, .T. ) ;
#9943 = CARTESIAN_POINT ( 'NONE',  ( 0.6866196799637447334, 0.03902977929019532666, 0.4282732318476364930 ) ) ;
#9944 = EDGE_CURVE ( 'NONE', #10100, #10863, #7173, .T. ) ;
#9945 = SHAPE_REPRESENTATION_RELATIONSHIP ( 'NONE' , 'NONE' ,  #1014, #14219 ) ;
#9946 = CARTESIAN_POINT ( 'NONE',  ( 0.6577550957999035441, -0.3830000000000000071, -0.4907096737881370130 ) ) ;
#9947 = ORIENTED_EDGE ( 'NONE', *, *, #15049, .T. ) ;
#9948 = AXIS2_PLACEMENT_3D ( 'NONE', #12980, #13970, #2513 ) ;
#9949 = CARTESIAN_POINT ( 'NONE',  ( 6.826491571325181695, 1.679378605318035733, -1.679378605318065487 ) ) ;
#9950 = CARTESIAN_POINT ( 'NONE',  ( 3.394491571325182644, 1.679378605318042395, -1.941878605318058337 ) ) ;
#9951 = DIRECTION ( 'NONE',  ( -1.000000000000000000, -0.000000000000000000, -0.000000000000000000 ) ) ;
#9952 = CIRCLE ( 'NONE', #3350, 1.000000000000000000 ) ;
#9953 = CARTESIAN_POINT ( 'NONE',  ( 0.6583850202313106248, -0.06301572931163962332, 0.5137832895838605474 ) ) ;
#9954 = CARTESIAN_POINT ( 'NONE',  ( 0.9705585225209942823, -0.4431353997581937709, -0.3488554439965182996 ) ) ;
#9955 = ORIENTED_EDGE ( 'NONE', *, *, #1277, .F. ) ;
#9956 = LINE ( 'NONE', #746, #13148 ) ;
#9957 = LINE ( 'NONE', #6295, #41 ) ;
#9958 = VECTOR ( 'NONE', #2812, 39.37007874015748143 ) ;
#9959 = CARTESIAN_POINT ( 'NONE',  ( 8.469665986256828205, 1.056999999999999940, 6.829619984160658046E-17 ) ) ;
#9960 = ORIENTED_EDGE ( 'NONE', *, *, #602, .F. ) ;
#9961 = PRODUCT ( 'Hex Bolt', 'Hex Bolt', '', ( #10923 ) ) ;
#9962 = CARTESIAN_POINT ( 'NONE',  ( 3.958564149947915389, 0.8698990160032655794, -0.4932443601560797530 ) ) ;
#9963 = DIRECTION ( 'NONE',  ( 0.000000000000000000, 0.000000000000000000, -1.000000000000000000 ) ) ;
#9964 = ORIENTED_EDGE ( 'NONE', *, *, #5236, .T. ) ;
#9965 = CARTESIAN_POINT ( 'NONE',  ( 2.774999999999999911, 2.360000000000016307, 0.9799999999999454703 ) ) ;
#9966 = ORIENTED_EDGE ( 'NONE', *, *, #775, .T. ) ;
#9967 = ADVANCED_FACE ( 'NONE', ( #14188 ), #8169, .T. ) ;
#9968 = DIRECTION ( 'NONE',  ( 0.000000000000000000, 0.000000000000000000, -1.000000000000000000 ) ) ;
#9969 = AXIS2_PLACEMENT_3D ( 'NONE', #12953, #10751, #2326 ) ;
#9970 = DIRECTION ( 'NONE',  ( 0.000000000000000000, 0.000000000000000000, -1.000000000000000000 ) ) ;
#9971 = DIRECTION ( 'NONE',  ( 0.000000000000000000, 0.000000000000000000, -1.000000000000000000 ) ) ;
#9972 = DIRECTION ( 'NONE',  ( 1.000000000000000000, 0.000000000000000000, 0.000000000000000000 ) ) ;
#9973 = ORIENTED_EDGE ( 'NONE', *, *, #2162, .T. ) ;
#9974 = AXIS2_PLACEMENT_3D ( 'NONE', #6169, #8469, #6242 ) ;
#9975 = FACE_OUTER_BOUND ( 'NONE', #14388, .T. ) ;
#9976 = CARTESIAN_POINT ( 'NONE',  ( 2.045495128834867060, 0.3295048711651352713, -0.4105035982572216580 ) ) ;
#9977 = VECTOR ( 'NONE', #8037, 39.37007874015748143 ) ;
#9978 =( REPRESENTATION_RELATIONSHIP ('NONE','NONE', #3591, #9930 ) REPRESENTATION_RELATIONSHIP_WITH_TRANSFORMATION ( #191 )SHAPE_REPRESENTATION_RELATIONSHIP( ) );
#9979 = LINE ( 'NONE', #9627, #1044 ) ;
#9980 = ORIENTED_EDGE ( 'NONE', *, *, #6525, .F. ) ;
#9981 = EDGE_LOOP ( 'NONE', ( #3351, #3201, #10292, #12600 ) ) ;
#9982 = ADVANCED_FACE ( 'NONE', ( #8094 ), #2342, .F. ) ;
#9983 = ORIENTED_EDGE ( 'NONE', *, *, #2991, .F. ) ;
#9984 = EDGE_CURVE ( 'NONE', #8675, #906, #11678, .T. ) ;
#9985 = CARTESIAN_POINT ( 'NONE',  ( 8.517841687953392693, 0.8704007761502546847, -0.3197150928555233529 ) ) ;
#9986 = ORIENTED_EDGE ( 'NONE', *, *, #14297, .T. ) ;
#9987 = EDGE_CURVE ( 'NONE', #1342, #11081, #13185, .T. ) ;
#9988 = CARTESIAN_POINT ( 'NONE',  ( 0.000000000000000000, 1.159999999999999698, -0.3190000000000000058 ) ) ;
#9989 = VECTOR ( 'NONE', #11731, 39.37007874015748143 ) ;
#9990 = CARTESIAN_POINT ( 'NONE',  ( 0.6609716345676606153, -0.4492731296520721673, -0.4835254040074319359 ) ) ;
#9991 = AXIS2_PLACEMENT_3D ( 'NONE', #9185, #12693, #8045 ) ;
#9992 = PLANE ( 'NONE',  #3411 ) ;
#9993 = AXIS2_PLACEMENT_3D ( 'NONE', #11729, #1224, #910 ) ;
#9994 = ADVANCED_FACE ( 'NONE', ( #12047 ), #12655, .F. ) ;
#9995 = CARTESIAN_POINT ( 'NONE',  ( 2.774999999999999911, 1.575000000000016387, 2.359999999999999876 ) ) ;
#9996 = EDGE_LOOP ( 'NONE', ( #13473, #4202, #11795, #844 ) ) ;
#9997 = AXIS2_PLACEMENT_3D ( 'NONE', #8118, #6969, #9418 ) ;
#9998 = VECTOR ( 'NONE', #8518, 39.37007874015748143 ) ;
#9999 = COLOUR_RGB ( '',0.7921568627450980005, 0.8196078431372548767, 0.9333333333333333481 ) ;
#10000 = VERTEX_POINT ( 'NONE', #13327 ) ;
#10001 = ORIENTED_EDGE ( 'NONE', *, *, #12294, .F. ) ;
#10002 = AXIS2_PLACEMENT_3D ( 'NONE', #1648, #8628, #5416 ) ;
#10003 = AXIS2_PLACEMENT_3D ( 'NONE', #13331, #5100, #14649 ) ;
#10004 = ORIENTED_EDGE ( 'NONE', *, *, #2656, .F. ) ;
#10005 = FACE_OUTER_BOUND ( 'NONE', #377, .T. ) ;
#10006 = CARTESIAN_POINT ( 'NONE',  ( 2.774999999999999911, 0.9799999999999436939, -3.360000000000016751 ) ) ;
#10007 = CARTESIAN_POINT ( 'NONE',  ( 4.205202298494868707, 0.9267662340798809018, 0.3758042580177037850 ) ) ;
#10008 = DIRECTION ( 'NONE',  ( 0.000000000000000000, 0.000000000000000000, 1.000000000000000000 ) ) ;
#10009 = ORIENTED_EDGE ( 'NONE', *, *, #14787, .F. ) ;
#10010 = DIRECTION ( 'NONE',  ( 1.000000000000000000, 0.000000000000000000, 0.000000000000000000 ) ) ;
#10011 = CARTESIAN_POINT ( 'NONE',  ( 8.280000379048722224E-17, 0.2159999999999999420, 0.7057575716915831521 ) ) ;
#10012 = DIRECTION ( 'NONE',  ( -1.000000000000000000, 0.000000000000000000, 0.000000000000000000 ) ) ;
#10013 = DIRECTION ( 'NONE',  ( 0.000000000000000000, 1.000000000000000000, -1.836536466328828134E-14 ) ) ;
#10014 = EDGE_CURVE ( 'NONE', #2874, #2357, #5096, .T. ) ;
#10015 = CIRCLE ( 'NONE', #14647, 0.2624999999999997335 ) ;
#10016 = CYLINDRICAL_SURFACE ( 'NONE', #11879, 0.8000000000000000444 ) ;
#10017 = CARTESIAN_POINT ( 'NONE',  ( 0.9484310486901441628, -0.4761373899265420317, -0.4326466961088093477 ) ) ;
#10018 = ADVANCED_FACE ( 'NONE', ( #6317 ), #11924, .F. ) ;
#10019 = CARTESIAN_POINT ( 'NONE',  ( 3.843202652328518987, 1.810746292266676605, 0.7496334864260736364 ) ) ;
#10021 = ORIENTED_EDGE ( 'NONE', *, *, #4977, .F. ) ;
#10020 = DIRECTION ( 'NONE',  ( 0.000000000000000000, 0.000000000000000000, -1.000000000000000000 ) ) ;
#10022 = ORIENTED_EDGE ( 'NONE', *, *, #2741, .F. ) ;
#10024 = VERTEX_POINT ( 'NONE', #2866 ) ;
#10023 = CARTESIAN_POINT ( 'NONE',  ( 3.876560711617219823, 1.855806856933289506, -0.7500000000000001110 ) ) ;
#10025 = ORIENTED_EDGE ( 'NONE', *, *, #12713, .T. ) ;
#10026 = VECTOR ( 'NONE', #12324, 39.37007874015748143 ) ;
#10027 = CARTESIAN_POINT ( 'NONE',  ( 0.000000000000000000, 1.239999999999999991, -0.4849999999999999312 ) ) ;
#10028 = CARTESIAN_POINT ( 'NONE',  ( -0.2249147617188397563, 1.239999999999999991, 0.3723417112827376307 ) ) ;
#10029 = ORIENTED_EDGE ( 'NONE', *, *, #1835, .F. ) ;
#10030 = DIRECTION ( 'NONE',  ( 1.000000000000000000, 0.000000000000000000, 0.000000000000000000 ) ) ;
#10031 = CARTESIAN_POINT ( 'NONE',  ( 2.775039370078740131, -1.679378605318048390, 2.054378605318054607 ) ) ;
#10032 = DIRECTION ( 'NONE',  ( 0.000000000000000000, 8.723548215061523903E-15, 1.000000000000000000 ) ) ;
#10033 = CARTESIAN_POINT ( 'NONE',  ( 0.8999999999999998002, 0.1549999999999996103, -0.3799999999999999489 ) ) ;
#10034 = EDGE_CURVE ( 'NONE', #2642, #1422, #6555, .T. ) ;
#10035 = ORIENTED_EDGE ( 'NONE', *, *, #2107, .T. ) ;
#10036 = ADVANCED_FACE ( 'NONE', ( #5023 ), #9689, .F. ) ;
#10037 = FACE_OUTER_BOUND ( 'NONE', #8389, .T. ) ;
#10038 = CARTESIAN_POINT ( 'NONE',  ( 3.469135854992689616, 0.9563780235308655397, -0.2924688362345267967 ) ) ;
#10039 = CARTESIAN_POINT ( 'NONE',  ( 3.944129661530210385, 1.761538328845252188, -0.7935532608319411096 ) ) ;
#10040 = EDGE_LOOP ( 'NONE', ( #8988, #6187, #2811, #8293 ) ) ;
#10041 = CARTESIAN_POINT ( 'NONE',  ( 0.06299999999999998657, 2.296825071800860970E-16, 1.875500000000000167 ) ) ;
#10042 = DIRECTION ( 'NONE',  ( 0.000000000000000000, 0.000000000000000000, 1.000000000000000000 ) ) ;
#10043 = ORIENTED_EDGE ( 'NONE', *, *, #10203, .F. ) ;
#10044 = CARTESIAN_POINT ( 'NONE',  ( 3.874999999999999556, 3.567999999999999616, -1.320000000000000062 ) ) ;
#10045 = ORIENTED_EDGE ( 'NONE', *, *, #12708, .F. ) ;
#10046 = COLOUR_RGB ( '',0.7921568627450980005, 0.8196078431372548767, 0.9333333333333333481 ) ;
#10047 = CARTESIAN_POINT ( 'NONE',  ( 3.713442968092242946, 1.916698194283638079, -0.7331915495002455652 ) ) ;
#10048 =( LENGTH_UNIT ( ) NAMED_UNIT ( * ) SI_UNIT ( $, .METRE. ) );
#10049 = FACE_OUTER_BOUND ( 'NONE', #14573, .T. ) ;
#10050 = CARTESIAN_POINT ( 'NONE',  ( 3.944129661530210385, 0.000000000000000000, 0.000000000000000000 ) ) ;
#10051 = EDGE_LOOP ( 'NONE', ( #7847, #3773, #2592, #6457 ) ) ;
#10052 = LINE ( 'NONE', #4238, #5025 ) ;
#10053 = CIRCLE ( 'NONE', #2227, 0.4070000000000044138 ) ;
#10054 = CARTESIAN_POINT ( 'NONE',  ( 3.875000000000000000, 3.137999999999999901, 0.000000000000000000 ) ) ;
#10055 = CARTESIAN_POINT ( 'NONE',  ( 6.826491571325181695, -1.679378605318047946, -1.679378605318053497 ) ) ;
#10056 = ORIENTED_EDGE ( 'NONE', *, *, #8956, .T. ) ;
#10057 = ORIENTED_EDGE ( 'NONE', *, *, #5323, .F. ) ;
#10058 = DIRECTION ( 'NONE',  ( 0.000000000000000000, -1.224646799147353454E-16, 1.000000000000000000 ) ) ;
#10059 = ORIENTED_EDGE ( 'NONE', *, *, #12529, .T. ) ;
#10060 = CARTESIAN_POINT ( 'NONE',  ( 0.000000000000000000, 1.109999999999999876, 0.000000000000000000 ) ) ;
#10061 = LINE ( 'NONE', #10287, #1739 ) ;
#10062 = AXIS2_PLACEMENT_3D ( 'NONE', #5712, #9545, #10373 ) ;
#10063 = DIRECTION ( 'NONE',  ( -0.000000000000000000, -1.000000000000000000, -0.000000000000000000 ) ) ;
#10064 = CARTESIAN_POINT ( 'NONE',  ( 4.626513628950617907, 1.810550457394507040, 0.04993882545213381569 ) ) ;
#10065 = EDGE_CURVE ( 'NONE', #5917, #9754, #14258, .T. ) ;
#10066 = ORIENTED_EDGE ( 'NONE', *, *, #6414, .T. ) ;
#10067 = EDGE_CURVE ( 'NONE', #12843, #14153, #3794, .T. ) ;
#10068 = CIRCLE ( 'NONE', #13960, 0.2624999999999994560 ) ;
#10069 = CARTESIAN_POINT ( 'NONE',  ( 4.268616971210836830, 1.710660744896744578, -0.6914058754706146059 ) ) ;
#10070 = ORIENTED_EDGE ( 'NONE', *, *, #11892, .T. ) ;
#10071 = ORIENTED_EDGE ( 'NONE', *, *, #3342, .F. ) ;
#10072 = EDGE_CURVE ( 'NONE', #12211, #4169, #1653, .T. ) ;
#10073 = ORIENTED_EDGE ( 'NONE', *, *, #3887, .F. ) ;
#10074 = LINE ( 'NONE', #4335, #6047 ) ;
#10075 = CARTESIAN_POINT ( 'NONE',  ( 0.6179999999999965521, -1.679378605318047946, -2.054378605318054163 ) ) ;
#10076 = CARTESIAN_POINT ( 'NONE',  ( 3.405153689607044232, 3.137999999999999901, -1.491010071662831171 ) ) ;
#10077 = LINE ( 'NONE', #8927, #11690 ) ;
#10078 = ORIENTED_EDGE ( 'NONE', *, *, #11565, .F. ) ;
#10079 = LINE ( 'NONE', #14734, #11182 ) ;
#10080 = DIRECTION ( 'NONE',  ( 0.3420201433256623846, 0.000000000000000000, 0.9396926207859106484 ) ) ;
#10081 = DIRECTION ( 'NONE',  ( -0.000000000000000000, -9.182682331643740718E-16, 1.000000000000000000 ) ) ;
#10082 = DIRECTION ( 'NONE',  ( 0.2251194151855832049, -0.9743259920144012876, 0.003179652756858328440 ) ) ;
#10083 = EDGE_CURVE ( 'NONE', #14802, #14728, #7532, .T. ) ;
#10084 = PRODUCT_DEFINITION_SHAPE ( 'NONE', 'NONE',  #15155 ) ;
#10085 = EDGE_CURVE ( 'NONE', #12293, #6203, #4014, .T. ) ;
#10086 = CIRCLE ( 'NONE', #3487, 0.3190000000000000058 ) ;
#10087 = FACE_OUTER_BOUND ( 'NONE', #4789, .T. ) ;
#10088 = CIRCLE ( 'NONE', #13978, 0.1899999999999999745 ) ;
#10089 = DIRECTION ( 'NONE',  ( -0.000000000000000000, -1.000000000000000000, -0.000000000000000000 ) ) ;
#10090 = CARTESIAN_POINT ( 'NONE',  ( 4.364820037892395810, 1.707069359036963219, 0.6292106624328539510 ) ) ;
#10092 = ORIENTED_EDGE ( 'NONE', *, *, #10633, .T. ) ;
#10091 = CARTESIAN_POINT ( 'NONE',  ( 3.827923612805795184, 1.898876434569533256, -0.4983202096988793017 ) ) ;
#10093 = ORIENTED_EDGE ( 'NONE', *, *, #10391, .F. ) ;
#10095 = ORIENTED_EDGE ( 'NONE', *, *, #7365, .F. ) ;
#10094 = DIRECTION ( 'NONE',  ( 0.000000000000000000, 0.000000000000000000, -1.000000000000000000 ) ) ;
#10096 = ORIENTED_EDGE ( 'NONE', *, *, #3796, .T. ) ;
#10097 = ADVANCED_FACE ( 'NONE', ( #472 ), #5836, .F. ) ;
#10098 = DIRECTION ( 'NONE',  ( 0.000000000000000000, 0.000000000000000000, 1.000000000000000000 ) ) ;
#10099 = DIRECTION ( 'NONE',  ( 0.000000000000000000, 0.000000000000000000, -1.000000000000000000 ) ) ;
#10100 = VERTEX_POINT ( 'NONE', #13254 ) ;
#10101 = DIRECTION ( 'NONE',  ( 1.000000000000000000, 0.000000000000000000, 0.000000000000000000 ) ) ;
#10102 = CARTESIAN_POINT ( 'NONE',  ( 2.124999999999999556, -1.679378605318041950, 1.679378605318059048 ) ) ;
#10103 = EDGE_CURVE ( 'NONE', #13854, #11243, #10460, .T. ) ;
#10104 = CARTESIAN_POINT ( 'NONE',  ( 3.099256572624759176, 0.9349522984524822888, -0.4562251896521926642 ) ) ;
#10105 = CARTESIAN_POINT ( 'NONE',  ( 1.008061589492043719, -0.4429852717212066637, -0.3350037431595069282 ) ) ;
#10106 = ORIENTED_EDGE ( 'NONE', *, *, #7113, .T. ) ;
#10107 = DIRECTION ( 'NONE',  ( 0.9999002670844989726, 0.000000000000000000, -0.01412288512831216640 ) ) ;
#10108 = CIRCLE ( 'NONE', #3508, 0.7849999999999958122 ) ;
#10109 = LINE ( 'NONE', #7654, #4464 ) ;
#10110 = CARTESIAN_POINT ( 'NONE',  ( 4.500934089278993078, 1.710778234005743359, -0.5029489024355867643 ) ) ;
#10111 = EDGE_CURVE ( 'NONE', #10542, #9681, #7300, .T. ) ;
#10112 = CIRCLE ( 'NONE', #1058, 1.350000000000000089 ) ;
#10113 = CARTESIAN_POINT ( 'NONE',  ( 0.7058998964907862161, -0.3830000000000000071, 0.4900296624789436950 ) ) ;
#10114 = DIRECTION ( 'NONE',  ( 0.000000000000000000, 0.000000000000000000, -1.000000000000000000 ) ) ;
#10115 = ORIENTED_EDGE ( 'NONE', *, *, #3047, .F. ) ;
#10116 = DIRECTION ( 'NONE',  ( 0.9999002670844991947, -2.602203049398214110E-17, 0.01412288512831213171 ) ) ;
#10117 = ORIENTED_EDGE ( 'NONE', *, *, #4221, .T. ) ;
#10118 = FACE_OUTER_BOUND ( 'NONE', #5146, .T. ) ;
#10119 = EDGE_CURVE ( 'NONE', #4965, #4727, #437, .T. ) ;
#10120 = AXIS2_PLACEMENT_3D ( 'NONE', #15065, #7954, #5591 ) ;
#10121 = DIRECTION ( 'NONE',  ( 0.000000000000000000, 1.000000000000000000, -0.000000000000000000 ) ) ;
#10122 =( GEOMETRIC_REPRESENTATION_CONTEXT ( 3 ) GLOBAL_UNCERTAINTY_ASSIGNED_CONTEXT ( ( #5405 ) ) GLOBAL_UNIT_ASSIGNED_CONTEXT ( ( #6729, #807, #735 ) ) REPRESENTATION_CONTEXT ( 'NONE', 'WORKASPACE' ) );
#10123 = FACE_OUTER_BOUND ( 'NONE', #8341, .T. ) ;
#10124 = CARTESIAN_POINT ( 'NONE',  ( 2.774999999999999911, -0.9799999999999436939, 2.360000000000016307 ) ) ;
#10125 = CARTESIAN_POINT ( 'NONE',  ( 0.4108223460329304411, 5.750000472440944144, -0.2849999999999985323 ) ) ;
#10126 = ORIENTED_EDGE ( 'NONE', *, *, #4633, .T. ) ;
#10127 = CARTESIAN_POINT ( 'NONE',  ( 2.774999999999999911, -1.679378605318041950, 1.973878605318058810 ) ) ;
#10128 = CARTESIAN_POINT ( 'NONE',  ( 3.760599021723662450, 1.814825219489536678, 0.7947699344343004402 ) ) ;
#10129 = VECTOR ( 'NONE', #9645, 39.37007874015748143 ) ;
#10130 = DIRECTION ( 'NONE',  ( -1.874307916738606601E-16, 1.000000000000000000, 0.000000000000000000 ) ) ;
#10131 = ORIENTED_EDGE ( 'NONE', *, *, #3934, .F. ) ;
#10132 = VERTEX_POINT ( 'NONE', #6995 ) ;
#10133 = CARTESIAN_POINT ( 'NONE',  ( 2.774999999999999911, 1.679378605318042395, -1.679378605318058604 ) ) ;
#10134 = ORIENTED_EDGE ( 'NONE', *, *, #14233, .F. ) ;
#10135 = DIRECTION ( 'NONE',  ( 1.000000000000000000, 0.000000000000000000, 0.000000000000000000 ) ) ;
#10136 = CARTESIAN_POINT ( 'NONE',  ( 2.124999999999999556, 1.679378605318042395, -1.384878605318058842 ) ) ;
#10137 = EDGE_CURVE ( 'NONE', #14777, #7182, #13929, .T. ) ;
#10138 = CARTESIAN_POINT ( 'NONE',  ( 3.426491571325181340, 0.000000000000000000, 0.000000000000000000 ) ) ;
#10139 = CONICAL_SURFACE ( 'NONE', #14770, 0.3750000000000007772, 0.7853981633974557175 ) ;
#10140 = CARTESIAN_POINT ( 'NONE',  ( 3.900033994830720552, 1.848181875390886519, -0.7500000000000002220 ) ) ;
#10141 = CIRCLE ( 'NONE', #3546, 0.04000000000000006328 ) ;
#10142 = ORIENTED_EDGE ( 'NONE', *, *, #3575, .T. ) ;
#10143 = ORIENTED_EDGE ( 'NONE', *, *, #11568, .F. ) ;
#10144 = ORIENTED_EDGE ( 'NONE', *, *, #5256, .T. ) ;
#10145 = UNCERTAINTY_MEASURE_WITH_UNIT (LENGTH_MEASURE( 1.000000000000000082E-05 ), #4491, 'distance_accuracy_value', 'NONE');
#10146 = AXIS2_PLACEMENT_3D ( 'NONE', #11467, #6654, #10099 ) ;
#10147 = ORIENTED_EDGE ( 'NONE', *, *, #4853, .T. ) ;
#10148 = CARTESIAN_POINT ( 'NONE',  ( 0.000000000000000000, 0.1749999999999999889, -0.8000000000000000444 ) ) ;
#10149 = AXIS2_PLACEMENT_3D ( 'NONE', #11743, #1315, #7992 ) ;
#10150 = CIRCLE ( 'NONE', #4539, 0.4999999999999997224 ) ;
#10151 = CARTESIAN_POINT ( 'NONE',  ( 3.426491571325181340, 2.062169880637645836, -0.5999481385559802815 ) ) ;
#10152 = CARTESIAN_POINT ( 'NONE',  ( 0.8712764764800380313, -1.315297834523746934, -0.4276878505061766922 ) ) ;
#10153 = LINE ( 'NONE', #5643, #6815 ) ;
#10154 = ORIENTED_EDGE ( 'NONE', *, *, #9164, .T. ) ;
#10155 = CARTESIAN_POINT ( 'NONE',  ( 2.837768005214870382, 0.5663408804686755893, 0.4003582515643820394 ) ) ;
#10156 = DIRECTION ( 'NONE',  ( -0.9999002670844991947, -1.607565641772518678E-17, 0.01412288512831583534 ) ) ;
#10157 = CARTESIAN_POINT ( 'NONE',  ( 8.474190026735612946, 0.9289129992088663856, 0.3203020658980472168 ) ) ;
#10158 = AXIS2_PLACEMENT_3D ( 'NONE', #4854, #7081, #14317 ) ;
#10159 = AXIS2_PLACEMENT_3D ( 'NONE', #9501, #352, #14367 ) ;
#10160 = B_SPLINE_CURVE_WITH_KNOTS ( 'NONE', 3,
 ( #11047, #6395, #1630, #474, #12426, #6546, #8839, #9830, #2795, #11206, #4016, #2946, #544, #14564, #13410, #6467, #707, #4177, #14485, #5398, #4096, #8762, #1708, #8685, #6321, #6246, #10064, #7609, #10982, #7535, #4250, #8913, #1781, #13256, #13559, #3101, #5170, #10907, #11126, #624, #7467, #5319, #399, #9763, #12125, #11584, #4632, #9068, #15024, #936, #5551, #1087, #1012, #13643, #10140, #8997 ),
 .UNSPECIFIED., .F., .F.,
 ( 4, 2, 2, 2, 2, 2, 2, 2, 2, 2, 2, 2, 2, 2, 2, 2, 2, 2, 2, 2, 2, 2, 2, 2, 2, 2, 2, 4 ),
 ( 0.01335241406472727557, 0.01712285003613359807, 0.01900806802183678534, 0.01995067701468835816, 0.02089328600753993098, 0.02466372197894622920, 0.02654893996464938177, 0.02843415795035252741, 0.03220459392175881175, 0.03408981190746195045, 0.03597502989316508915, 0.03786024787886822784, 0.03974546586457137348, 0.04351590183597766476, 0.04540111982168081040, 0.04728633780738396297, 0.05105677377879025425, 0.05294199176449340682, 0.05482720975019655940, 0.05671242773589969810, 0.05859764572160285068, 0.06236808169300916971, 0.06425329967871233616, 0.06519590867156389857, 0.06613851766441547486, 0.06990895363582165511, 0.07179417162152473830, 0.07367938960722780761 ),
 .UNSPECIFIED. ) ;
#10161 = CARTESIAN_POINT ( 'NONE',  ( 0.9065573155407952166, -0.4416294641957835831, -0.4501509288694744981 ) ) ;
#10162 = CARTESIAN_POINT ( 'NONE',  ( 4.145336115082029593, 1.743003941933530587, 0.7011725378991962021 ) ) ;
#10164 = ORIENTED_EDGE ( 'NONE', *, *, #10574, .T. ) ;
#10163 = CARTESIAN_POINT ( 'NONE',  ( 0.000000000000000000, 1.629999999999999893, -0.2432499999999999385 ) ) ;
#10165 = EDGE_LOOP ( 'NONE', ( #9983, #4788, #14490, #14597 ) ) ;
#10167 = EDGE_LOOP ( 'NONE', ( #11654, #7056, #7473, #7242 ) ) ;
#10166 = CARTESIAN_POINT ( 'NONE',  ( 3.405153689607044232, 2.750000000000000000, -1.491010071662831171 ) ) ;
#10168 = VERTEX_POINT ( 'NONE', #6146 ) ;
#10169 = EDGE_CURVE ( 'NONE', #6943, #1935, #4376, .T. ) ;
#10170 = EDGE_CURVE ( 'NONE', #12552, #11912, #5105, .T. ) ;
#10171 = DIRECTION ( 'NONE',  ( -0.3420201433256623846, 0.000000000000000000, -0.9396926207859106484 ) ) ;
#10172 = AXIS2_PLACEMENT_3D ( 'NONE', #7966, #8968, #12394 ) ;
#10173 = DIRECTION ( 'NONE',  ( -1.000000000000000000, -0.000000000000000000, -0.000000000000000000 ) ) ;
#10174 = EDGE_LOOP ( 'NONE', ( #3317, #10022, #3240, #5386, #77, #10021, #11841, #2609, #14495, #10915, #3835, #5175, #7848, #1620, #14251, #7982, #12852, #4384, #7495, #11738, #5464, #6398, #1701, #8086, #11652 ) ) ;
#10175 = EDGE_CURVE ( 'NONE', #1037, #4626, #8304, .T. ) ;
#10176 = LINE ( 'NONE', #11621, #7707 ) ;
#10177 = FACE_OUTER_BOUND ( 'NONE', #1322, .T. ) ;
#10178 = CIRCLE ( 'NONE', #4528, 0.5000000000000000000 ) ;
#10179 = AXIS2_PLACEMENT_3D ( 'NONE', #11505, #8907, #5696 ) ;
#10180 = LINE ( 'NONE', #1130, #13520 ) ;
#10181 = EDGE_CURVE ( 'NONE', #1151, #4018, #12186, .T. ) ;
#10182 =( REPRESENTATION_RELATIONSHIP ('NONE','NONE', #3591, #1600 ) REPRESENTATION_RELATIONSHIP_WITH_TRANSFORMATION ( #13423 )SHAPE_REPRESENTATION_RELATIONSHIP( ) );
#10183 = CARTESIAN_POINT ( 'NONE',  ( 2.957700166090663885, 0.9550922613677363948, -0.4582245739254896533 ) ) ;
#10184 = CARTESIAN_POINT ( 'NONE',  ( 0.9682536368877157074, -0.4829999999707417224, -0.3433101715744485971 ) ) ;
#10185 = ORIENTED_EDGE ( 'NONE', *, *, #11564, .T. ) ;
#10186 = VECTOR ( 'NONE', #10618, 39.37007874015748143 ) ;
#10187 = DIRECTION ( 'NONE',  ( -1.000000000000000000, -0.000000000000000000, -0.000000000000000000 ) ) ;
#10188 = CARTESIAN_POINT ( 'NONE',  ( 3.544798737392580001, 0.9267668399616416641, -0.3758007328785020196 ) ) ;
#10189 = CARTESIAN_POINT ( 'NONE',  ( 6.208491571325183145, 1.679378605318059492, 2.054378605318042172 ) ) ;
#10190 = FACE_OUTER_BOUND ( 'NONE', #7167, .T. ) ;
#10191 = CIRCLE ( 'NONE', #7271, 0.03999999999999999389 ) ;
#10192 = CARTESIAN_POINT ( 'NONE',  ( 0.4124999999999997558, -0.6590000000000000302, -0.4125000000000000333 ) ) ;
#10193 = ORIENTED_EDGE ( 'NONE', *, *, #13054, .T. ) ;
#10194 = CARTESIAN_POINT ( 'NONE',  ( 2.774999999999999911, -0.6999999999999990674, -2.399999999999999911 ) ) ;
#10195 = AXIS2_PLACEMENT_3D ( 'NONE', #12134, #7615, #1713 ) ;
#10196 = CARTESIAN_POINT ( 'NONE',  ( 0.7727406610312560487, 0.1749999999999999889, -0.2070552360820117899 ) ) ;
#10197 = CARTESIAN_POINT ( 'NONE',  ( 3.426491571325181340, -0.9799999999999989830, -2.359999999999999876 ) ) ;
#10198 = CARTESIAN_POINT ( 'NONE',  ( 0.2812500000000000555, 1.249999999999999778, 0.000000000000000000 ) ) ;
#10199 = EDGE_CURVE ( 'NONE', #10875, #2564, #12917, .T. ) ;
#10200 = VERTEX_POINT ( 'NONE', #14237 ) ;
#10201 = DIRECTION ( 'NONE',  ( 1.000000000000000000, 0.000000000000000000, 0.000000000000000000 ) ) ;
#10202 = DIRECTION ( 'NONE',  ( 0.000000000000000000, 0.000000000000000000, -1.000000000000000000 ) ) ;
#10203 = EDGE_CURVE ( 'NONE', #2606, #5449, #1908, .T. ) ;
#10204 = CARTESIAN_POINT ( 'NONE',  ( 3.875000000000000000, 3.535499999999999865, 0.000000000000000000 ) ) ;
#10205 = ORIENTED_EDGE ( 'NONE', *, *, #6372, .F. ) ;
#10206 = ORIENTED_EDGE ( 'NONE', *, *, #11689, .T. ) ;
#10207 = DIRECTION ( 'NONE',  ( 0.000000000000000000, 0.000000000000000000, -1.000000000000000000 ) ) ;
#10208 = CARTESIAN_POINT ( 'NONE',  ( 3.874999999999999556, 3.170500000000001428, -1.320000000000000062 ) ) ;
#10209 = EDGE_LOOP ( 'NONE', ( #1137, #6152, #2832, #14476 ) ) ;
#10210 = CARTESIAN_POINT ( 'NONE',  ( 2.156999999999999584, 1.679378605318059048, 1.941878605318041240 ) ) ;
#10211 = AXIS2_PLACEMENT_3D ( 'NONE', #5737, #13744, #9261 ) ;
#10212 = CARTESIAN_POINT ( 'NONE',  ( 0.6555286510801260347, -0.4026824885229741136, -0.5099168278768623219 ) ) ;
#10213 = CARTESIAN_POINT ( 'NONE',  ( 0.6179999999999962190, -1.679378605318048390, 1.304378605318053497 ) ) ;
#10214 = CARTESIAN_POINT ( 'NONE',  ( 6.787121492585022509, 0.000000000000000000, 0.000000000000000000 ) ) ;
#10215 = B_SPLINE_CURVE_WITH_KNOTS ( 'NONE', 3,
 ( #10279, #14711, #4239, #10347, #6682, #10128, #5689, #14780, #3091, #6532, #12477, #4315 ),
 .UNSPECIFIED., .F., .F.,
 ( 4, 2, 2, 2, 2, 4 ),
 ( 0.000000000000000000, 0.001826406838012980009, 0.003652813676025960018, 0.007305627352051886209, 0.01095844102807781197, 0.01461125470410373599 ),
 .UNSPECIFIED. ) ;
#10216 = ORIENTED_EDGE ( 'NONE', *, *, #12833, .T. ) ;
#10217 = VECTOR ( 'NONE', #8871, 39.37007874015748143 ) ;
#10218 = EDGE_CURVE ( 'NONE', #11004, #5653, #6829, .T. ) ;
#10219 = VERTEX_POINT ( 'NONE', #9294 ) ;
#10220 = ORIENTED_EDGE ( 'NONE', *, *, #3548, .F. ) ;
#10221 = DIRECTION ( 'NONE',  ( 0.000000000000000000, 0.000000000000000000, 1.000000000000000000 ) ) ;
#10222 = VERTEX_POINT ( 'NONE', #4768 ) ;
#10223 = AXIS2_PLACEMENT_3D ( 'NONE', #14418, #7462, #13111 ) ;
#10224 = DIRECTION ( 'NONE',  ( -0.000000000000000000, 0.000000000000000000, 1.000000000000000000 ) ) ;
#10225 = CARTESIAN_POINT ( 'NONE',  ( 3.394491571325183088, 1.679378605318059048, 1.679378605318041506 ) ) ;
#10227 = FACE_BOUND ( 'NONE', #8528, .T. ) ;
#10226 = AXIS2_PLACEMENT_3D ( 'NONE', #9868, #7804, #7576 ) ;
#10228 = CARTESIAN_POINT ( 'NONE',  ( 2.280218097287834311, 0.5641718375782867057, 0.4677935296993194214 ) ) ;
#10229 = ORIENTED_EDGE ( 'NONE', *, *, #11770, .T. ) ;
#10230 = LINE ( 'NONE', #13956, #8537 ) ;
#10231 = FACE_OUTER_BOUND ( 'NONE', #5309, .T. ) ;
#10232 = CARTESIAN_POINT ( 'NONE',  ( 2.743000000000000327, 1.679378605318042395, -1.679378605318058604 ) ) ;
#10233 = CIRCLE ( 'NONE', #5595, 2.500000000000000444 ) ;
#10234 = AXIS2_PLACEMENT_3D ( 'NONE', #13160, #7369, #4062 ) ;
#10235 = AXIS2_PLACEMENT_3D ( 'NONE', #3772, #2312, #8445 ) ;
#10236 = DIRECTION ( 'NONE',  ( -0.000000000000000000, -1.000000000000000000, -0.000000000000000000 ) ) ;
#10237 = AXIS2_PLACEMENT_3D ( 'NONE', #8551, #8257, #4956 ) ;
#10238 = EDGE_CURVE ( 'NONE', #8364, #13702, #5342, .T. ) ;
#10239 = CARTESIAN_POINT ( 'NONE',  ( 4.004051897178946717, 1.768001349219448626, 0.7400188025467686614 ) ) ;
#10241 = EDGE_LOOP ( 'NONE', ( #11986, #1034, #10396, #13402 ) ) ;
#10240 = DIRECTION ( 'NONE',  ( -1.000000000000000000, -0.000000000000000000, -0.000000000000000000 ) ) ;
#10242 = ORIENTED_EDGE ( 'NONE', *, *, #3461, .F. ) ;
#10244 = ORIENTED_EDGE ( 'NONE', *, *, #13372, .F. ) ;
#10243 = CARTESIAN_POINT ( 'NONE',  ( 0.000000000000000000, 1.591999999999999638, 0.000000000000000000 ) ) ;
#10245 = VERTEX_POINT ( 'NONE', #8144 ) ;
#10246 = FACE_OUTER_BOUND ( 'NONE', #8751, .T. ) ;
#10247 = CARTESIAN_POINT ( 'NONE',  ( 0.007908111413600218964, -0.2214999999999999469, 0.5598942880828960966 ) ) ;
#10248 = ORIENTED_EDGE ( 'NONE', *, *, #10635, .T. ) ;
#10249 = AXIS2_PLACEMENT_3D ( 'NONE', #6673, #4385, #7515 ) ;
#10250 = CARTESIAN_POINT ( 'NONE',  ( 0.000000000000000000, 0.000000000000000000, 0.000000000000000000 ) ) ;
#10251 = DIRECTION ( 'NONE',  ( 0.7071067811865462405, -0.7071067811865489050, 0.000000000000000000 ) ) ;
#10252 = AXIS2_PLACEMENT_3D ( 'NONE', #11680, #1186, #14114 ) ;
#10253 = CARTESIAN_POINT ( 'NONE',  ( 0.3725000000000000533, 0.1749999999999999889, 0.3724999999999999978 ) ) ;
#10254 = CARTESIAN_POINT ( 'NONE',  ( 3.874999999999999556, 2.750000000000000000, -1.320000000000000062 ) ) ;
#10255 = CARTESIAN_POINT ( 'NONE',  ( 2.418884559267300727, 0.5995087936326214395, -0.4658349638521568359 ) ) ;
#10256 = EDGE_CURVE ( 'NONE', #4101, #6363, #8042, .T. ) ;
#10257 = CARTESIAN_POINT ( 'NONE',  ( 8.661818191809109280, 0.8754285464536269989, 0.3176815264168136865 ) ) ;
#10258 = EDGE_CURVE ( 'NONE', #3105, #7033, #10659, .T. ) ;
#10259 = ORIENTED_EDGE ( 'NONE', *, *, #8615, .F. ) ;
#10260 = EDGE_CURVE ( 'NONE', #12467, #504, #7542, .T. ) ;
#10261 = DIRECTION ( 'NONE',  ( 0.4961857140186716753, -0.000000000000000000, 0.8682164115033652596 ) ) ;
#10262 = CARTESIAN_POINT ( 'NONE',  ( 3.829348296951585073, 1.894867393789687160, 0.4984412668866745055 ) ) ;
#10263 = DIRECTION ( 'NONE',  ( 1.000000000000000000, 0.000000000000000000, 0.000000000000000000 ) ) ;
#10264 = AXIS2_PLACEMENT_3D ( 'NONE', #772, #8081, #8911 ) ;
#10265 = CARTESIAN_POINT ( 'NONE',  ( 6.208491571325183145, -1.679378605318047946, -1.679378605318053497 ) ) ;
#10267 = EDGE_LOOP ( 'NONE', ( #5926, #8479, #13041, #9919 ) ) ;
#10266 = CARTESIAN_POINT ( 'NONE',  ( 3.875000000000000000, 3.535499999999999865, -0.4849999999999995981 ) ) ;
#10268 = ORIENTED_EDGE ( 'NONE', *, *, #2698, .T. ) ;
#10269 = ADVANCED_FACE ( 'NONE', ( #13087 ), #15109, .F. ) ;
#10270 = CARTESIAN_POINT ( 'NONE',  ( -0.03836742111524548554, 0.6316479427872651042, -0.4405359281558275941 ) ) ;
#10271 = CARTESIAN_POINT ( 'NONE',  ( 2.124999999999999556, -1.679378605318059048, -1.973878605318026613 ) ) ;
#10272 = LINE ( 'NONE', #14928, #13505 ) ;
#10273 = CARTESIAN_POINT ( 'NONE',  ( -0.7435009325572419225, -0.6334543218446815338, -9.105260372192982189E-17 ) ) ;
#10274 = DIRECTION ( 'NONE',  ( 0.000000000000000000, 0.000000000000000000, 1.000000000000000000 ) ) ;
#10275 = ADVANCED_FACE ( 'NONE', ( #12944 ), #8769, .F. ) ;
#10276 = DIRECTION ( 'NONE',  ( 1.000000000000000000, 0.000000000000000000, 3.491481338843132961E-15 ) ) ;
#10277 = ORIENTED_EDGE ( 'NONE', *, *, #1243, .T. ) ;
#10278 = CARTESIAN_POINT ( 'NONE',  ( 0.000000000000000000, 0.1749999999999999889, 0.000000000000000000 ) ) ;
#10279 = CARTESIAN_POINT ( 'NONE',  ( 3.944129661530210385, 1.761538328845252188, 0.7935532608319412207 ) ) ;
#10280 = CARTESIAN_POINT ( 'NONE',  ( 0.09035531712817643224, 1.629999999999999893, 0.1564999999999999447 ) ) ;
#10281 = ORIENTED_EDGE ( 'NONE', *, *, #13877, .F. ) ;
#10282 = CARTESIAN_POINT ( 'NONE',  ( -0.3725000000000002198, -0.6590000000000000302, -0.3725000000000000533 ) ) ;
#10283 = CARTESIAN_POINT ( 'NONE',  ( 2.001999999999999780, 1.726751986797767896E-16, 1.409999999999999920 ) ) ;
#10284 = EDGE_LOOP ( 'NONE', ( #7214, #4123, #5445, #13791 ) ) ;
#10285 = CARTESIAN_POINT ( 'NONE',  ( 2.592367411162172619, 0.4049457270506669482, 0.4633846410852800468 ) ) ;
#10286 = EDGE_CURVE ( 'NONE', #11264, #1773, #8052, .T. ) ;
#10287 = CARTESIAN_POINT ( 'NONE',  ( 0.000000000000000000, 0.000000000000000000, -0.3190000000000000058 ) ) ;
#10288 = CARTESIAN_POINT ( 'NONE',  ( 0.6500000000000001332, 1.901497511147140416E-16, -1.552690549202460968 ) ) ;
#10289 = EDGE_CURVE ( 'NONE', #4855, #5394, #1382, .T. ) ;
#10290 = CARTESIAN_POINT ( 'NONE',  ( 2.774999999999999911, -2.400000000000011902, -0.6999999999999596545 ) ) ;
#10291 =( GEOMETRIC_REPRESENTATION_CONTEXT ( 3 ) GLOBAL_UNCERTAINTY_ASSIGNED_CONTEXT ( ( #4480 ) ) GLOBAL_UNIT_ASSIGNED_CONTEXT ( ( #321, #11983, #12326 ) ) REPRESENTATION_CONTEXT ( 'NONE', 'WORKASPACE' ) );
#10292 = ORIENTED_EDGE ( 'NONE', *, *, #499, .F. ) ;
#10293 = ORIENTED_EDGE ( 'NONE', *, *, #4684, .T. ) ;
#10294 = ORIENTED_EDGE ( 'NONE', *, *, #11655, .F. ) ;
#10295 = CARTESIAN_POINT ( 'NONE',  ( -0.4312750580175238602, 1.564824237736551771, -0.01491519342844984525 ) ) ;
#10296 = ORIENTED_EDGE ( 'NONE', *, *, #1651, .F. ) ;
#10297 = CIRCLE ( 'NONE', #16, 1.000000000000000666 ) ;
#10298 = DIRECTION ( 'NONE',  ( -1.000000000000000000, 0.000000000000000000, 0.000000000000000000 ) ) ;
#10299 = CYLINDRICAL_SURFACE ( 'NONE', #6772, 0.4349999999999999423 ) ;
#10300 = CARTESIAN_POINT ( 'NONE',  ( 0.7905038590255393238, -0.4446454637884403871, -0.3161764760585322187 ) ) ;
#10301 = CARTESIAN_POINT ( 'NONE',  ( 2.187203820042824098, 0.4712135623730924205, 0.4085020630706684974 ) ) ;
#10302 = ORIENTED_EDGE ( 'NONE', *, *, #9018, .T. ) ;
#10303 = CARTESIAN_POINT ( 'NONE',  ( 4.769268701363833074, 3.137999999999999901, 0.3249191361593796734 ) ) ;
#10304 = EDGE_CURVE ( 'NONE', #12746, #5546, #10738, .T. ) ;
#10305 = EDGE_CURVE ( 'NONE', #11081, #12243, #3153, .T. ) ;
#10306 = CARTESIAN_POINT ( 'NONE',  ( 0.6583927779709175532, -0.06304930530161369229, -0.5137831800632942647 ) ) ;
#10307 = DIRECTION ( 'NONE',  ( 0.000000000000000000, 0.000000000000000000, -1.000000000000000000 ) ) ;
#10308 = CIRCLE ( 'NONE', #7153, 0.2624999999999852451 ) ;
#10309 = CYLINDRICAL_SURFACE ( 'NONE', #9371, 0.5000000000000001110 ) ;
#10310 = CARTESIAN_POINT ( 'NONE',  ( 4.626188208514882660, 1.723983726829047214, 0.2983432309202477817 ) ) ;
#10312 = ORIENTED_EDGE ( 'NONE', *, *, #3781, .T. ) ;
#10311 = CARTESIAN_POINT ( 'NONE',  ( 3.390179639970223313, 0.6913388717410868800, 0.3921396980529558429 ) ) ;
#10313 = ORIENTED_EDGE ( 'NONE', *, *, #13239, .T. ) ;
#10315 = ORIENTED_EDGE ( 'NONE', *, *, #1257, .T. ) ;
#10314 = CARTESIAN_POINT ( 'NONE',  ( 3.876560711617219379, 3.137999999999999901, 0.000000000000000000 ) ) ;
#10316 = VERTEX_POINT ( 'NONE', #8520 ) ;
#10317 = LINE ( 'NONE', #15057, #9498 ) ;
#10318 = CARTESIAN_POINT ( 'NONE',  ( 0.8999999999999999112, -0.6230000000000016636, -0.2999999999999999889 ) ) ;
#10319 = EDGE_LOOP ( 'NONE', ( #9694, #7912, #1019, #10029 ) ) ;
#10320 = CARTESIAN_POINT ( 'NONE',  ( 0.5816197779170538817, 0.000000000000000000, -1.650520655410200099 ) ) ;
#10321 = CARTESIAN_POINT ( 'NONE',  ( 8.474191475755167957, 0.8688764771518150409, -0.3203316212763323567 ) ) ;
#10322 = EDGE_CURVE ( 'NONE', #3025, #8103, #14392, .T. ) ;
#10323 = CYLINDRICAL_SURFACE ( 'NONE', #9138, 0.1250000000000000278 ) ;
#10324 = DIRECTION ( 'NONE',  ( -0.000000000000000000, -1.000000000000000000, -0.000000000000000000 ) ) ;
#10325 = FACE_OUTER_BOUND ( 'NONE', #3216, .T. ) ;
#10326 = AXIS2_PLACEMENT_3D ( 'NONE', #12314, #14918, #13752 ) ;
#10327 = DIRECTION ( 'NONE',  ( 0.000000000000000000, 1.000000000000000000, -0.000000000000000000 ) ) ;
#10328 = FACE_OUTER_BOUND ( 'NONE', #12674, .T. ) ;
#10329 = PLANE ( 'NONE',  #10967 ) ;
#10330 = CARTESIAN_POINT ( 'NONE',  ( 4.134613691807048852, 1.724441890029780211, -0.7513151844660320711 ) ) ;
#10331 = DIRECTION ( 'NONE',  ( -0.7071067811865429098, 0.000000000000000000, 0.7071067811865521247 ) ) ;
#10333 = ORIENTED_EDGE ( 'NONE', *, *, #5978, .F. ) ;
#10332 = CARTESIAN_POINT ( 'NONE',  ( 3.944129661530210385, 2.407784495501249742E-16, -1.932031071636253650 ) ) ;
#10334 = MANIFOLD_SOLID_BREP ( 'Fillet4', #549 ) ;
#10335 = ORIENTED_EDGE ( 'NONE', *, *, #1084, .T. ) ;
#10336 = CARTESIAN_POINT ( 'NONE',  ( 3.601417382415921686, 0.9969999999999999973, -0.3891265382754440227 ) ) ;
#10337 = EDGE_LOOP ( 'NONE', ( #13614, #4276, #3014, #9351, #6354, #8841, #14786, #14320, #3452, #7660, #10470, #11501, #695 ) ) ;
#10338 = EDGE_CURVE ( 'NONE', #9926, #9226, #5601, .T. ) ;
#10339 = SPHERICAL_SURFACE ( 'NONE', #701, 0.8499999999999999778 ) ;
#10340 = CARTESIAN_POINT ( 'NONE',  ( 2.917021349547980424, 0.5710164562864796789, -0.4587991334809999877 ) ) ;
#10341 = CARTESIAN_POINT ( 'NONE',  ( 0.6894988814560869539, -0.4425276619544661894, -0.4465617225471331664 ) ) ;
#10342 = DIRECTION ( 'NONE',  ( -1.000000000000000000, -0.000000000000000000, -0.000000000000000000 ) ) ;
#10343 = VECTOR ( 'NONE', #11112, 39.37007874015748143 ) ;
#10344 = CARTESIAN_POINT ( 'NONE',  ( 0.09500000000000168032, 0.000000000000000000, 0.000000000000000000 ) ) ;
#10345 = EDGE_LOOP ( 'NONE', ( #1120, #8378, #4729, #4047 ) ) ;
#10346 = DIRECTION ( 'NONE',  ( 1.655665450705613915E-16, 3.103226861728128995E-32, 1.000000000000000000 ) ) ;
#10347 = CARTESIAN_POINT ( 'NONE',  ( 3.851668032307324463, 1.786355384972422966, 0.7987671621174978753 ) ) ;
#10348 = VERTEX_POINT ( 'NONE', #2767 ) ;
#10349 = DIRECTION ( 'NONE',  ( 0.000000000000000000, 0.000000000000000000, -1.000000000000000000 ) ) ;
#10350 = ORIENTED_EDGE ( 'NONE', *, *, #2611, .F. ) ;
#10351 = DIRECTION ( 'NONE',  ( 0.000000000000000000, -0.7071067811865595631, 0.7071067811865354713 ) ) ;
#10352 = LINE ( 'NONE', #14011, #1784 ) ;
#10353 = ORIENTED_EDGE ( 'NONE', *, *, #13537, .F. ) ;
#10354 = AXIS2_PLACEMENT_3D ( 'NONE', #11393, #2127, #8193 ) ;
#10355 = CARTESIAN_POINT ( 'NONE',  ( 3.096478849372236386, 0.7064487239733231450, 0.4562644230314655824 ) ) ;
#10356 = EDGE_CURVE ( 'NONE', #12826, #1005, #12093, .T. ) ;
#10357 = AXIS2_PLACEMENT_3D ( 'NONE', #7513, #10960, #6077 ) ;
#10358 = LINE ( 'NONE', #8316, #2573 ) ;
#10359 = ADVANCED_FACE ( 'NONE', ( #9663, #448 ), #1604, .F. ) ;
#10360 = ADVANCED_FACE ( 'NONE', ( #7583 ), #1750, .F. ) ;
#10361 = CARTESIAN_POINT ( 'NONE',  ( 0.8276409636798741642, -0.4389750926356451033, -0.4504658872936693204 ) ) ;
#10362 = DIRECTION ( 'NONE',  ( 0.000000000000000000, 0.000000000000000000, -1.000000000000000000 ) ) ;
#10363 = EDGE_CURVE ( 'NONE', #3778, #8716, #9747, .T. ) ;
#10364 = VECTOR ( 'NONE', #926, 39.37007874015748143 ) ;
#10365 = CARTESIAN_POINT ( 'NONE',  ( 6.794491571325181667, 1.679378605318059492, 1.304378605318041062 ) ) ;
#10366 = ADVANCED_FACE ( 'NONE', ( #13453 ), #14630, .F. ) ;
#10367 = CARTESIAN_POINT ( 'NONE',  ( 4.011028178682179757, 1.745898953245868412, -0.7846266810094224553 ) ) ;
#10368 = ORIENTED_EDGE ( 'NONE', *, *, #11010, .F. ) ;
#10369 = ORIENTED_EDGE ( 'NONE', *, *, #14550, .T. ) ;
#10370 = CARTESIAN_POINT ( 'NONE',  ( 2.774999999999999911, 1.679378605318042395, -1.416878605318059314 ) ) ;
#10371 = VERTEX_POINT ( 'NONE', #7371 ) ;
#10372 = CARTESIAN_POINT ( 'NONE',  ( 2.774999999999999911, -2.400000000000011902, -0.6999999999999596545 ) ) ;
#10373 = DIRECTION ( 'NONE',  ( 0.3420201433256623846, 0.000000000000000000, -0.9396926207859106484 ) ) ;
#10374 = DIRECTION ( 'NONE',  ( 0.7071067811865459074, -0.7071067811865492381, 0.000000000000000000 ) ) ;
#10375 = CIRCLE ( 'NONE', #6968, 0.8653656741516848605 ) ;
#10376 = CYLINDRICAL_SURFACE ( 'NONE', #12408, 0.3750000000000004996 ) ;
#10377 = EDGE_LOOP ( 'NONE', ( #4890, #983 ) ) ;
#10378 = CARTESIAN_POINT ( 'NONE',  ( 3.182018581797185774, 2.483907847764145416, 0.2845129745686012512 ) ) ;
#10379 = CARTESIAN_POINT ( 'NONE',  ( 0.6940259540059535714, 0.04143956037114119445, -0.4146509415068644899 ) ) ;
#10380 = DIRECTION ( 'NONE',  ( 0.000000000000000000, 0.000000000000000000, 1.000000000000000000 ) ) ;
#10381 = EDGE_CURVE ( 'NONE', #9226, #12391, #9734, .T. ) ;
#10382 = EDGE_CURVE ( 'NONE', #11155, #969, #372, .T. ) ;
#10383 = SURFACE_STYLE_FILL_AREA ( #5722 ) ;
#10384 = AXIS2_PLACEMENT_3D ( 'NONE', #3357, #14828, #11242 ) ;
#10385 = CARTESIAN_POINT ( 'NONE',  ( 4.518491583832497938, 1.735549304995126718, -0.3882790969652222812 ) ) ;
#10386 = EDGE_LOOP ( 'NONE', ( #4124, #2585, #6975, #3423, #13307 ) ) ;
#10387 = VECTOR ( 'NONE', #12631, 39.37007874015748854 ) ;
#10389 = ORIENTED_EDGE ( 'NONE', *, *, #13267, .T. ) ;
#10388 = LINE ( 'NONE', #1265, #6931 ) ;
#10390 = CIRCLE ( 'NONE', #14288, 0.8083085967350902568 ) ;
#10391 = EDGE_CURVE ( 'NONE', #5805, #1313, #7312, .T. ) ;
#10392 = VERTEX_POINT ( 'NONE', #3114 ) ;
#10394 = ORIENTED_EDGE ( 'NONE', *, *, #3047, .T. ) ;
#10393 = LINE ( 'NONE', #11614, #871 ) ;
#10395 =( BOUNDED_SURFACE ( )  B_SPLINE_SURFACE ( 3, 2, ( 
 ( #2761, #8725, #9800 ),
 ( #9953, #9872, #7364 ),
 ( #2692, #4992, #14607 ),
 ( #7429, #6433, #2985 ),
 ( #14452, #3919, #4142 ),
 ( #8582, #1819, #14525 ),
 ( #9658, #13296, #5206 ),
 ( #13222, #3981, #2837 ),
 ( #8513, #6211, #12087 ),
 ( #13156, #13367, #6290 ),
 ( #2917, #366, #5068 ),
 ( #10946, #7578, #290 ),
 ( #441, #12164, #6366 ),
 ( #12017, #5142, #8651 ),
 ( #10873, #14307, #1678 ),
 ( #11019, #3842, #10800 ) ),
 .UNSPECIFIED., .F., .F., .F. ) 
 B_SPLINE_SURFACE_WITH_KNOTS ( ( 4, 2, 2, 2, 2, 2, 2, 4 ),
 ( 3, 3 ),
 ( 0.002083263661281777729, 0.002712596804664463811, 0.003341929948047149893, 0.003971263091429835974, 0.004600596234812522056, 0.005229929378195208138, 0.005859262521577894220, 0.007117928808343267251 ),
 ( 0.000000000000000000, 1.000000000000000000 ),
 .UNSPECIFIED. ) 
 GEOMETRIC_REPRESENTATION_ITEM ( )  RATIONAL_B_SPLINE_SURFACE ( (
 ( 1.000000000000000000, 0.8987017906623451236, 1.000000000000000000),
 ( 1.000000000000000000, 0.9020594141852221748, 1.000000000000000000),
 ( 1.000000000000000000, 0.9044651860912357177, 1.000000000000000000),
 ( 1.000000000000000000, 0.9073335834958523582, 1.000000000000000000),
 ( 1.000000000000000000, 0.9077660037302067719, 1.000000000000000000),
 ( 1.000000000000000000, 0.9065807100087762693, 1.000000000000000000),
 ( 1.000000000000000000, 0.9049576633627300914, 1.000000000000000000),
 ( 1.000000000000000000, 0.8998093858009506008, 1.000000000000000000),
 ( 1.000000000000000000, 0.8963317359660779582, 1.000000000000000000),
 ( 1.000000000000000000, 0.8876325024793222385, 1.000000000000000000),
 ( 1.000000000000000000, 0.8824894405371271899, 1.000000000000000000),
 ( 1.000000000000000000, 0.8708860455746204599, 1.000000000000000000),
 ( 1.000000000000000000, 0.8643359190951755977, 1.000000000000000000),
 ( 1.000000000000000000, 0.8432203508675353287, 1.000000000000000000),
 ( 1.000000000000000000, 0.8269334966168219170, 1.000000000000000000),
 ( 1.000000000000000000, 0.8091170061680454939, 1.000000000000000000) ) ) 
 REPRESENTATION_ITEM ( '' )  SURFACE ( )  );
#10396 = ORIENTED_EDGE ( 'NONE', *, *, #975, .F. ) ;
#10397 = CARTESIAN_POINT ( 'NONE',  ( 2.527624975756972425, 2.750000000000000000, -0.9199802545633498640 ) ) ;
#10398 = FACE_OUTER_BOUND ( 'NONE', #3358, .T. ) ;
#10399 = ORIENTED_EDGE ( 'NONE', *, *, #9944, .F. ) ;
#10400 = DIRECTION ( 'NONE',  ( 0.000000000000000000, 0.000000000000000000, -1.000000000000000000 ) ) ;
#10401 = DIRECTION ( 'NONE',  ( 1.000000000000000000, 0.000000000000000000, 0.000000000000000000 ) ) ;
#10402 = AXIS2_PLACEMENT_3D ( 'NONE', #3544, #8229, #7157 ) ;
#10403 = CARTESIAN_POINT ( 'NONE',  ( 0.000000000000000000, 1.239999999999999991, 0.000000000000000000 ) ) ;
#10404 = DIRECTION ( 'NONE',  ( -0.000000000000000000, -1.000000000000000000, 0.000000000000000000 ) ) ;
#10405 = AXIS2_PLACEMENT_3D ( 'NONE', #4136, #8802, #11244 ) ;
#10406 = VECTOR ( 'NONE', #9349, 39.37007874015748854 ) ;
#10407 = DIRECTION ( 'NONE',  ( 0.7071067811865450192, -0.7071067811865501263, 0.000000000000000000 ) ) ;
#10408 = DIRECTION ( 'NONE',  ( 0.000000000000000000, 0.000000000000000000, 1.000000000000000000 ) ) ;
#10409 = DIRECTION ( 'NONE',  ( -0.000000000000000000, -0.000000000000000000, -1.000000000000000000 ) ) ;
#10410 = CARTESIAN_POINT ( 'NONE',  ( 3.479169036718512409, 0.9521518695376113284, 0.3059096338091180645 ) ) ;
#10411 = CARTESIAN_POINT ( 'NONE',  ( 4.181805601875195677, 1.718400334928297468, 0.7333929193435403393 ) ) ;
#10412 = EDGE_CURVE ( 'NONE', #3646, #8801, #12088, .T. ) ;
#10413 = AXIS2_PLACEMENT_3D ( 'NONE', #14620, #1831, #4154 ) ;
#10414 = DIRECTION ( 'NONE',  ( -1.000000000000000000, 0.000000000000000000, 0.000000000000000000 ) ) ;
#10416 = ORIENTED_EDGE ( 'NONE', *, *, #7591, .F. ) ;
#10415 = CARTESIAN_POINT ( 'NONE',  ( 0.6500000000000001332, 1.679378605318059492, 2.086378605318045754 ) ) ;
#10417 = EDGE_LOOP ( 'NONE', ( #14412, #4941, #12530, #5716 ) ) ;
#10418 = AXIS2_PLACEMENT_3D ( 'NONE', #3407, #1654, #11067 ) ;
#10419 = CARTESIAN_POINT ( 'NONE',  ( 0.09035531712817643224, 1.379999999999999671, 0.1564999999999999447 ) ) ;
#10420 = ORIENTED_EDGE ( 'NONE', *, *, #10382, .F. ) ;
#10421 = CARTESIAN_POINT ( 'NONE',  ( 2.124999999999999556, -1.679378605318059048, -1.384878605318057510 ) ) ;
#10422 = VECTOR ( 'NONE', #5729, 39.37007874015748143 ) ;
#10423 = DIRECTION ( 'NONE',  ( -1.000000000000000000, -0.000000000000000000, -0.000000000000000000 ) ) ;
#10424 = CARTESIAN_POINT ( 'NONE',  ( 0.000000000000000000, 0.1749999999999999889, 0.000000000000000000 ) ) ;
#10425 = EDGE_LOOP ( 'NONE', ( #1078, #10056, #12058, #3473 ) ) ;
#10426 = CARTESIAN_POINT ( 'NONE',  ( 3.496294824931886147, 1.921163641483014439, -0.7211466812414543126 ) ) ;
#10427 = LINE ( 'NONE', #10657, #14229 ) ;
#10428 = EDGE_LOOP ( 'NONE', ( #7920, #5654, #12474, #11426 ) ) ;
#10429 = CARTESIAN_POINT ( 'NONE',  ( 3.405153689607044232, 3.137999999999999901, 1.491010071662831171 ) ) ;
#10430 = ADVANCED_FACE ( 'NONE', ( #11364 ), #2259, .T. ) ;
#10431 = ORIENTED_EDGE ( 'NONE', *, *, #14383, .T. ) ;
#10432 = AXIS2_PLACEMENT_3D ( 'NONE', #10679, #2420, #7103 ) ;
#10433 = DIRECTION ( 'NONE',  ( 0.9659258262890698665, 0.000000000000000000, -0.2588190451025147443 ) ) ;
#10434 = ORIENTED_EDGE ( 'NONE', *, *, #8353, .T. ) ;
#10435 = PLANE ( 'NONE',  #13305 ) ;
#10436 = VECTOR ( 'NONE', #3888, 39.37007874015748143 ) ;
#10437 = CARTESIAN_POINT ( 'NONE',  ( 1.519298119451390150, -0.3788322150374328068, -0.4785409870133183752 ) ) ;
#10438 = FACE_OUTER_BOUND ( 'NONE', #5678, .T. ) ;
#10439 = FACE_OUTER_BOUND ( 'NONE', #6163, .T. ) ;
#10440 = AXIS2_PLACEMENT_3D ( 'NONE', #9465, #15110, #5936 ) ;
#10441 = CARTESIAN_POINT ( 'NONE',  ( 2.774999999999999911, 1.679378605318059048, 1.679378605318041506 ) ) ;
#10442 = EDGE_CURVE ( 'NONE', #2908, #8125, #9265, .T. ) ;
#10443 = ADVANCED_FACE ( 'NONE', ( #7926 ), #2920, .F. ) ;
#10444 = ADVANCED_FACE ( 'NONE', ( #866, #9233 ), #2020, .T. ) ;
#10445 = CARTESIAN_POINT ( 'NONE',  ( 3.722375483330346846, 1.851882672529376439, -0.7344444148597581989 ) ) ;
#10446 = ORIENTED_EDGE ( 'NONE', *, *, #10169, .F. ) ;
#10447 = EDGE_LOOP ( 'NONE', ( #4351, #14958 ) ) ;
#10448 = CARTESIAN_POINT ( 'NONE',  ( 3.426491571325181784, 2.050018311957429784, 0.6006734803707507453 ) ) ;
#10449 = ORIENTED_EDGE ( 'NONE', *, *, #14764, .T. ) ;
#10450 = DIRECTION ( 'NONE',  ( 0.000000000000000000, 0.000000000000000000, -1.000000000000000000 ) ) ;
#10451 = CARTESIAN_POINT ( 'NONE',  ( 2.003951500898715654, -0.1834701832127830778, 0.4716956002697921257 ) ) ;
#10452 = CARTESIAN_POINT ( 'NONE',  ( 0.000000000000000000, 0.1749999999999999889, 0.000000000000000000 ) ) ;
#10453 = EDGE_CURVE ( 'NONE', #13687, #9092, #2099, .T. ) ;
#10454 = CARTESIAN_POINT ( 'NONE',  ( 3.426491571325181340, -0.6999999999999989564, -2.399999999999999911 ) ) ;
#10455 = ORIENTED_EDGE ( 'NONE', *, *, #6197, .T. ) ;
#10456 = CARTESIAN_POINT ( 'NONE',  ( 0.7142320474717510637, -0.01055004872664746032, -0.4648272691893420294 ) ) ;
#10457 = LINE ( 'NONE', #11832, #7841 ) ;
#10458 = AXIS2_PLACEMENT_3D ( 'NONE', #1591, #14446, #6205 ) ;
#10459 = CARTESIAN_POINT ( 'NONE',  ( 0.8999999999999999112, -0.4829999999999998739, -0.3750000000000000555 ) ) ;
#10460 = CIRCLE ( 'NONE', #2890, 0.7849999999999992539 ) ;
#10461 = CARTESIAN_POINT ( 'NONE',  ( 4.662226822519125236, 1.729394697956203597, 0.1892339305778590608 ) ) ;
#10462 = ORIENTED_EDGE ( 'NONE', *, *, #11715, .T. ) ;
#10464 = EDGE_LOOP ( 'NONE', ( #8034, #7333, #14007, #781 ) ) ;
#10463 = CARTESIAN_POINT ( 'NONE',  ( 0.3480941905909775147, 1.602948811930423156, 0.1589886820288792801 ) ) ;
#10465 = CONICAL_SURFACE ( 'NONE', #13135, 0.2944999999999998175, 0.7853981633974536081 ) ;
#10466 =( REPRESENTATION_RELATIONSHIP ('NONE','NONE', #3591, #1600 ) REPRESENTATION_RELATIONSHIP_WITH_TRANSFORMATION ( #8850 )SHAPE_REPRESENTATION_RELATIONSHIP( ) );
#10467 = ORIENTED_EDGE ( 'NONE', *, *, #9608, .T. ) ;
#10469 = EDGE_LOOP ( 'NONE', ( #8085, #8908, #13503, #3972 ) ) ;
#10468 = CARTESIAN_POINT ( 'NONE',  ( 2.743000000000000771, 1.679378605318059048, 1.679378605318041506 ) ) ;
#10470 = ORIENTED_EDGE ( 'NONE', *, *, #1065, .T. ) ;
#10471 = CARTESIAN_POINT ( 'NONE',  ( 6.826491571325181695, 0.000000000000000000, 0.000000000000000000 ) ) ;
#10472 = CARTESIAN_POINT ( 'NONE',  ( 0.000000000000000000, 0.000000000000000000, 0.000000000000000000 ) ) ;
#10473 = DIRECTION ( 'NONE',  ( -0.000000000000000000, -1.000000000000000000, 0.000000000000000000 ) ) ;
#10474 = VERTEX_POINT ( 'NONE', #4565 ) ;
#10475 = VECTOR ( 'NONE', #1071, 39.37007874015748143 ) ;
#10476 = CARTESIAN_POINT ( 'NONE',  ( 2.001999999999999780, 0.000000000000000000, 0.000000000000000000 ) ) ;
#10477 = DIRECTION ( 'NONE',  ( 0.9992912762382413216, 0.03489602031262311471, 0.01411428356268702201 ) ) ;
#10478 = AXIS2_PLACEMENT_3D ( 'NONE', #13982, #978, #5669 ) ;
#10479 = EDGE_CURVE ( 'NONE', #8413, #5428, #6635, .T. ) ;
#10480 = CARTESIAN_POINT ( 'NONE',  ( 3.794247516364918749, 1.884217686586828755, -0.7465934532251186084 ) ) ;
#10481 = VECTOR ( 'NONE', #14530, 39.37007874015748143 ) ;
#10482 = CARTESIAN_POINT ( 'NONE',  ( 2.774999999999999911, 0.6999999999999599876, -2.400000000000011458 ) ) ;
#10483 = VECTOR ( 'NONE', #10477, 39.37007874015748854 ) ;
#10484 = ADVANCED_FACE ( 'NONE', ( #6941, #10227, #12437, #13873, #3416, #715 ), #9154, .F. ) ;
#10485 = DIRECTION ( 'NONE',  ( -0.000000000000000000, -1.000000000000000000, -0.000000000000000000 ) ) ;
#10486 = ORIENTED_EDGE ( 'NONE', *, *, #10014, .T. ) ;
#10487 = LINE ( 'NONE', #13829, #1652 ) ;
#10488 = LINE ( 'NONE', #56, #9854 ) ;
#10489 = CARTESIAN_POINT ( 'NONE',  ( 4.394316455220915074, 1.707002683764069939, 0.6062743810478267159 ) ) ;
#10490 = B_SPLINE_CURVE_WITH_KNOTS ( 'NONE', 3,
 ( #13168, #2707, #13384, #14241, #8451, #7376, #14464, #8659, #14398, #1537, #6221, #10886, #12248, #2847 ),
 .UNSPECIFIED., .F., .F.,
 ( 4, 2, 2, 2, 2, 2, 4 ),
 ( 8.673617379884035472E-19, 0.0003612929182777952029, 0.0007225858365555895384, 0.001083878754833383874, 0.001445171673111178209, 0.002167757509666766880, 0.002890343346222355551 ),
 .UNSPECIFIED. ) ;
#10491 = EDGE_LOOP ( 'NONE', ( #466, #708, #3354, #5949 ) ) ;
#10492 = AXIS2_PLACEMENT_3D ( 'NONE', #829, #5528, #14848 ) ;
#10493 = FACE_OUTER_BOUND ( 'NONE', #505, .T. ) ;
#10495 = EDGE_LOOP ( 'NONE', ( #9835, #6435, #13485, #14973 ) ) ;
#10494 = CARTESIAN_POINT ( 'NONE',  ( 0.4108223460329302745, 0.000000000000000000, -0.2849999999999981992 ) ) ;
#10496 = ORIENTED_EDGE ( 'NONE', *, *, #5785, .T. ) ;
#10497 = DIRECTION ( 'NONE',  ( 0.000000000000000000, -1.000000000000000000, 0.000000000000000000 ) ) ;
#10498 = ORIENTED_EDGE ( 'NONE', *, *, #14962, .T. ) ;
#10499 = CARTESIAN_POINT ( 'NONE',  ( -5.764454660286586870E-18, -0.2214999999999999469, 0.000000000000000000 ) ) ;
#10500 = EDGE_CURVE ( 'NONE', #14149, #12577, #8785, .T. ) ;
#10501 = EDGE_CURVE ( 'NONE', #6554, #39, #8317, .T. ) ;
#10502 = LINE ( 'NONE', #7148, #7229 ) ;
#10503 = CONICAL_SURFACE ( 'NONE', #3907, 0.1520000000000001905, 0.7853981633974460586 ) ;
#10504 = LINE ( 'NONE', #15152, #9989 ) ;
#10505 = AXIS2_PLACEMENT_3D ( 'NONE', #9673, #1470, #9970 ) ;
#10506 = ORIENTED_EDGE ( 'NONE', *, *, #5133, .T. ) ;
#10507 = CARTESIAN_POINT ( 'NONE',  ( 0.6558154374103718487, -0.4244538358989483617, 0.5012742423172266149 ) ) ;
#10508 = DIRECTION ( 'NONE',  ( -1.000000000000000000, -0.000000000000000000, -0.000000000000000000 ) ) ;
#10509 = CARTESIAN_POINT ( 'NONE',  ( 3.875000000000000000, 1.112678268764263789, -0.5849999999999996314 ) ) ;
#10510 = ORIENTED_EDGE ( 'NONE', *, *, #9137, .T. ) ;
#10511 = DIRECTION ( 'NONE',  ( 0.000000000000000000, 1.000000000000000000, 0.000000000000000000 ) ) ;
#10512 = ORIENTED_EDGE ( 'NONE', *, *, #10218, .F. ) ;
#10513 = CARTESIAN_POINT ( 'NONE',  ( 3.875000000000000000, 1.059999999999999165, 0.000000000000000000 ) ) ;
#10514 = DIRECTION ( 'NONE',  ( 0.3420201433256623846, 0.000000000000000000, 0.9396926207859106484 ) ) ;
#10515 = ORIENTED_EDGE ( 'NONE', *, *, #700, .T. ) ;
#10516 = DIRECTION ( 'NONE',  ( 0.000000000000000000, -4.591341165822166182E-16, -1.000000000000000000 ) ) ;
#10517 = CIRCLE ( 'NONE', #3184, 1.932031071636253650 ) ;
#10518 = DIRECTION ( 'NONE',  ( 1.000000000000000000, 0.000000000000000000, 0.000000000000000000 ) ) ;
#10519 = DIRECTION ( 'NONE',  ( 0.000000000000000000, 0.000000000000000000, 1.000000000000000000 ) ) ;
#10520 = DIRECTION ( 'NONE',  ( -1.000000000000000000, -1.837151692781460616E-16, 0.000000000000000000 ) ) ;
#10521 = CARTESIAN_POINT ( 'NONE',  ( 3.543808504702383289, 1.925955906416788377, -0.6728280703062919921 ) ) ;
#10522 = VERTEX_POINT ( 'NONE', #5482 ) ;
#10523 = VERTEX_POINT ( 'NONE', #4261 ) ;
#10524 = DIRECTION ( 'NONE',  ( 0.000000000000000000, 0.000000000000000000, -1.000000000000000000 ) ) ;
#10525 = ORIENTED_EDGE ( 'NONE', *, *, #8710, .F. ) ;
#10526 = CARTESIAN_POINT ( 'NONE',  ( 8.789999999999999147, 1.056999999999999940, 6.829619984160658046E-17 ) ) ;
#10527 = PLANE ( 'NONE',  #14449 ) ;
#10528 =( NAMED_UNIT ( * ) PLANE_ANGLE_UNIT ( ) SI_UNIT ( $, .RADIAN. ) );
#10529 = LINE ( 'NONE', #10454, #3140 ) ;
#10530 = VERTEX_POINT ( 'NONE', #10076 ) ;
#10531 = AXIS2_PLACEMENT_3D ( 'NONE', #8258, #5795, #3730 ) ;
#10532 = CARTESIAN_POINT ( 'NONE',  ( 0.6500000000000001332, 0.000000000000000000, 1.552690549202460968 ) ) ;
#10533 = ADVANCED_FACE ( 'NONE', ( #7777 ), #4337, .F. ) ;
#10534 = DIRECTION ( 'NONE',  ( 0.000000000000000000, 1.000000000000000000, -0.000000000000000000 ) ) ;
#10535 = LINE ( 'NONE', #4723, #726 ) ;
#10536 = DIRECTION ( 'NONE',  ( 0.000000000000000000, 0.000000000000000000, -1.000000000000000000 ) ) ;
#10537 = ADVANCED_FACE ( 'NONE', ( #1102 ), #2423, .T. ) ;
#10538 = AXIS2_PLACEMENT_3D ( 'NONE', #7539, #547, #1303 ) ;
#10539 = CARTESIAN_POINT ( 'NONE',  ( 4.606889440629292842, 1.746155438930072856, -0.1743145812842641362 ) ) ;
#10540 = ORIENTED_EDGE ( 'NONE', *, *, #7363, .T. ) ;
#10542 = VERTEX_POINT ( 'NONE', #3859 ) ;
#10541 = CARTESIAN_POINT ( 'NONE',  ( 0.2285287788938192011, 1.564783867144734053, 0.3660820499162522612 ) ) ;
#10543 = VERTEX_POINT ( 'NONE', #5788 ) ;
#10544 = FACE_OUTER_BOUND ( 'NONE', #2415, .T. ) ;
#10545 = VERTEX_POINT ( 'NONE', #4643 ) ;
#10546 = FACE_OUTER_BOUND ( 'NONE', #7386, .T. ) ;
#10547 = DIRECTION ( 'NONE',  ( -2.081668171172168513E-17, -0.9826498540527065506, 0.1854703866664282330 ) ) ;
#10548 = CARTESIAN_POINT ( 'NONE',  ( 0.8249999999999999556, -0.4829999999999998739, -0.3750000000000000555 ) ) ;
#10549 = ORIENTED_EDGE ( 'NONE', *, *, #14930, .T. ) ;
#10550 = DIRECTION ( 'NONE',  ( -1.000000000000000000, -0.000000000000000000, -0.000000000000000000 ) ) ;
#10551 = CARTESIAN_POINT ( 'NONE',  ( 2.774999999999999911, -1.679378605318059048, -1.384878605318056399 ) ) ;
#10552 = ADVANCED_FACE ( 'NONE', ( #10888 ), #8663, .F. ) ;
#10553 = FACE_OUTER_BOUND ( 'NONE', #10337, .T. ) ;
#10554 = EDGE_CURVE ( 'NONE', #5034, #2332, #9275, .T. ) ;
#10555 = VECTOR ( 'NONE', #11752, 39.37007874015748143 ) ;
#10556 = DIRECTION ( 'NONE',  ( -1.000000000000000000, 0.000000000000000000, 0.000000000000000000 ) ) ;
#10557 = CARTESIAN_POINT ( 'NONE',  ( 0.2099999999999999922, 1.239999999999999991, 0.3809527529760087239 ) ) ;
#10558 = EDGE_CURVE ( 'NONE', #11081, #6020, #12030, .T. ) ;
#10559 = CARTESIAN_POINT ( 'NONE',  ( 3.841842303834268169, 0.8660254037844385966, 0.5000000000000003331 ) ) ;
#10560 = CARTESIAN_POINT ( 'NONE',  ( 4.484040318217246579, 1.709965233507263260, 0.5205613024012289980 ) ) ;
#10561 = ADVANCED_FACE ( 'NONE', ( #1253 ), #13308, .F. ) ;
#10562 = ORIENTED_EDGE ( 'NONE', *, *, #5796, .F. ) ;
#10563 = LINE ( 'NONE', #5673, #10885 ) ;
#10565 = ORIENTED_EDGE ( 'NONE', *, *, #2125, .T. ) ;
#10564 = CARTESIAN_POINT ( 'NONE',  ( 0.4124999999999999223, 0.1859999999999983611, 0.3724999999999999423 ) ) ;
#10566 = ORIENTED_EDGE ( 'NONE', *, *, #9463, .T. ) ;
#10567 = CARTESIAN_POINT ( 'NONE',  ( 2.774999999999999911, 1.377727649040770417E-16, 1.124999999999998446 ) ) ;
#10568 = FACE_OUTER_BOUND ( 'NONE', #9482, .T. ) ;
#10569 = ORIENTED_EDGE ( 'NONE', *, *, #10853, .F. ) ;
#10570 = CARTESIAN_POINT ( 'NONE',  ( 0.6179999999999965521, 1.679378605318035733, -1.679378605318065487 ) ) ;
#10571 = CIRCLE ( 'NONE', #13003, 0.4070000000000044138 ) ;
#10572 = DIRECTION ( 'NONE',  ( 0.000000000000000000, 0.000000000000000000, -1.000000000000000000 ) ) ;
#10573 = CARTESIAN_POINT ( 'NONE',  ( 0.8999999999999999112, -0.4429999999999998939, -0.3750000000000000555 ) ) ;
#10574 = EDGE_CURVE ( 'NONE', #2309, #14837, #13170, .T. ) ;
#10575 = ORIENTED_EDGE ( 'NONE', *, *, #356, .F. ) ;
#10576 = CARTESIAN_POINT ( 'NONE',  ( 3.411612174842781009, 2.070834547792271607, -0.5884920204652813736 ) ) ;
#10577 = CYLINDRICAL_SURFACE ( 'NONE', #4708, 0.2624999999999994560 ) ;
#10578 = AXIS2_PLACEMENT_3D ( 'NONE', #13350, #13663, #7559 ) ;
#10579 = CARTESIAN_POINT ( 'NONE',  ( 3.944129661530210385, 0.000000000000000000, 0.000000000000000000 ) ) ;
#10580 = ORIENTED_EDGE ( 'NONE', *, *, #14787, .T. ) ;
#10581 = DIRECTION ( 'NONE',  ( 0.000000000000000000, 0.000000000000000000, -1.000000000000000000 ) ) ;
#10582 = ORIENTED_EDGE ( 'NONE', *, *, #10500, .F. ) ;
#10583 = MECHANICAL_DESIGN_GEOMETRIC_PRESENTATION_REPRESENTATION (  '', ( #7892 ), #9119 ) ;
#10584 = ADVANCED_FACE ( 'NONE', ( #7442 ), #2849, .T. ) ;
#10585 = DIRECTION ( 'NONE',  ( -1.874307916738608820E-16, 1.000000000000000000, 0.000000000000000000 ) ) ;
#10586 = ORIENTED_EDGE ( 'NONE', *, *, #2307, .T. ) ;
#10587 = CARTESIAN_POINT ( 'NONE',  ( 6.208491571325183145, 1.679378605318035733, -1.679378605318065487 ) ) ;
#10588 = VECTOR ( 'NONE', #13850, 39.37007874015748143 ) ;
#10589 = CARTESIAN_POINT ( 'NONE',  ( 2.322097220811789597, 0.05061516561976652645, -0.4672020166538503050 ) ) ;
#10590 = CARTESIAN_POINT ( 'NONE',  ( -0.3725000000000000533, -0.6590000000000000302, 0.3724999999999999423 ) ) ;
#10591 = CARTESIAN_POINT ( 'NONE',  ( -0.4425000000000006706, 0.2159999999999999420, -0.3725000000000000533 ) ) ;
#10592 = AXIS2_PLACEMENT_3D ( 'NONE', #6191, #2743, #6755 ) ;
#10593 = ORIENTED_EDGE ( 'NONE', *, *, #5988, .T. ) ;
#10594 = ORIENTED_EDGE ( 'NONE', *, *, #11281, .F. ) ;
#10595 = ORIENTED_EDGE ( 'NONE', *, *, #7365, .T. ) ;
#10596 = VECTOR ( 'NONE', #10433, 39.37007874015748854 ) ;
#10597 = ADVANCED_FACE ( 'NONE', ( #8168 ), #9672, .T. ) ;
#10598 = CARTESIAN_POINT ( 'NONE',  ( 1.008069866910759504, -0.4429852340093067831, -0.3350284807826328093 ) ) ;
#10599 = CLOSED_SHELL ( 'NONE', ( #12057, #8883, #11682, #3633, #11312, #5493, #3011, #9640, #6533, #8855, #4691, #2776, #4752, #10991, #9274, #4194, #884, #3310, #6842, #4677, #10552, #4281, #14651, #10688 ) ) ;
#10600 = DIRECTION ( 'NONE',  ( -0.000000000000000000, -1.000000000000000000, -0.000000000000000000 ) ) ;
#10601 = CARTESIAN_POINT ( 'NONE',  ( 0.9652705920801474271, -0.4828330467331338749, -0.4119425203458967344 ) ) ;
#10602 = CARTESIAN_POINT ( 'NONE',  ( 0.3724999999999997757, -0.6290000000000004476, -0.4125000000000000333 ) ) ;
#10603 = FACE_OUTER_BOUND ( 'NONE', #11342, .T. ) ;
#10604 = ORIENTED_EDGE ( 'NONE', *, *, #3012, .T. ) ;
#10605 = CARTESIAN_POINT ( 'NONE',  ( 3.394491571325182644, 1.679378605318042395, -1.679378605318058604 ) ) ;
#10606 = DIRECTION ( 'NONE',  ( -1.000000000000000000, -1.689854595570744117E-16, 2.664535259100375303E-15 ) ) ;
#10607 = AXIS2_PLACEMENT_3D ( 'NONE', #7491, #7416, #12150 ) ;
#10608 = LINE ( 'NONE', #9239, #3936 ) ;
#10609 = MANIFOLD_SOLID_BREP ( 'Fillet4', #11324 ) ;
#10610 = CARTESIAN_POINT ( 'NONE',  ( 1.844710921988106378, 0.09661955516503979713, -0.4739447609888686741 ) ) ;
#10611 = CARTESIAN_POINT ( 'NONE',  ( 4.573675675097676141, 1.800317658760837158, -0.2789865180029196257 ) ) ;
#10612 = ORIENTED_EDGE ( 'NONE', *, *, #2856, .F. ) ;
#10614 = ORIENTED_EDGE ( 'NONE', *, *, #2195, .T. ) ;
#10613 = CARTESIAN_POINT ( 'NONE',  ( -0.2849999999999995315, 4.529999999999999361, 0.4108223460329293864 ) ) ;
#10615 = ORIENTED_EDGE ( 'NONE', *, *, #11407, .F. ) ;
#10616 = PRODUCT_RELATED_PRODUCT_CATEGORY ( 'part', '', ( #9961 ) ) ;
#10617 = AXIS2_PLACEMENT_3D ( 'NONE', #2680, #14291, #7351 ) ;
#10618 = DIRECTION ( 'NONE',  ( -0.000000000000000000, -1.000000000000000000, -0.000000000000000000 ) ) ;
#10619 = EDGE_LOOP ( 'NONE', ( #9966, #187, #7257, #11742 ) ) ;
#10620 = ORIENTED_EDGE ( 'NONE', *, *, #11283, .T. ) ;
#10621 = FACE_OUTER_BOUND ( 'NONE', #1563, .T. ) ;
#10622 = DIRECTION ( 'NONE',  ( 0.000000000000000000, 0.000000000000000000, 1.000000000000000000 ) ) ;
#10623 = VERTEX_POINT ( 'NONE', #9812 ) ;
#10624 = LINE ( 'NONE', #14137, #14342 ) ;
#10625 = DIRECTION ( 'NONE',  ( 0.000000000000000000, 0.000000000000000000, -1.000000000000000000 ) ) ;
#10626 = CARTESIAN_POINT ( 'NONE',  ( 3.426491571325181340, 2.062169880637645836, 0.5999481385559802815 ) ) ;
#10627 = AXIS2_PLACEMENT_3D ( 'NONE', #4467, #14226, #9139 ) ;
#10628 = DIRECTION ( 'NONE',  ( 0.000000000000000000, 0.000000000000000000, -1.000000000000000000 ) ) ;
#10629 = AXIS2_PLACEMENT_3D ( 'NONE', #10587, #14097, #12952 ) ;
#10630 = AXIS2_PLACEMENT_3D ( 'NONE', #12856, #1227, #10572 ) ;
#10631 = DIRECTION ( 'NONE',  ( -1.000000000000000000, -0.000000000000000000, -0.000000000000000000 ) ) ;
#10632 = DIRECTION ( 'NONE',  ( 0.000000000000000000, -0.000000000000000000, -1.000000000000000000 ) ) ;
#10633 = EDGE_CURVE ( 'NONE', #5151, #13738, #4148, .T. ) ;
#10634 = CARTESIAN_POINT ( 'NONE',  ( 4.669107278503995317, 1.730498534900028362, 0.1593143144689976309 ) ) ;
#10635 = EDGE_CURVE ( 'NONE', #4134, #15055, #4071, .T. ) ;
#10636 = ORIENTED_EDGE ( 'NONE', *, *, #9923, .T. ) ;
#10637 = EDGE_CURVE ( 'NONE', #287, #9235, #5380, .T. ) ;
#10638 = LINE ( 'NONE', #131, #5279 ) ;
#10640 = ORIENTED_EDGE ( 'NONE', *, *, #2184, .T. ) ;
#10639 = DIRECTION ( 'NONE',  ( 1.000000000000000000, 0.000000000000000000, 0.000000000000000000 ) ) ;
#10641 = MANIFOLD_SOLID_BREP ( 'Fillet1', #304 ) ;
#10642 = ORIENTED_EDGE ( 'NONE', *, *, #8454, .F. ) ;
#10643 = CARTESIAN_POINT ( 'NONE',  ( 6.176491571325181340, 0.000000000000000000, 0.000000000000000000 ) ) ;
#10644 = DIRECTION ( 'NONE',  ( -1.365923996832131609E-16, 1.000000000000000000, 0.000000000000000000 ) ) ;
#10645 = CARTESIAN_POINT ( 'NONE',  ( 0.000000000000000000, 0.000000000000000000, 0.000000000000000000 ) ) ;
#10646 = ORIENTED_EDGE ( 'NONE', *, *, #9367, .T. ) ;
#10647 = DIRECTION ( 'NONE',  ( -0.000000000000000000, -1.000000000000000000, -0.000000000000000000 ) ) ;
#10648 = CIRCLE ( 'NONE', #10149, 0.7406097974541305806 ) ;
#10649 = AXIS2_PLACEMENT_3D ( 'NONE', #60, #7136, #14994 ) ;
#10650 = ADVANCED_FACE ( 'NONE', ( #7662 ), #11178, .F. ) ;
#10651 = CARTESIAN_POINT ( 'NONE',  ( 3.426491571325181340, 0.9799999999999438050, -2.360000000000016307 ) ) ;
#10652 = CARTESIAN_POINT ( 'NONE',  ( 2.774999999999999911, -0.6999999999999598765, 2.400000000000012346 ) ) ;
#10653 = EDGE_LOOP ( 'NONE', ( #4024, #9307, #1968, #19 ) ) ;
#10654 = AXIS2_PLACEMENT_3D ( 'NONE', #5215, #7437, #10042 ) ;
#10655 = CARTESIAN_POINT ( 'NONE',  ( 0.2849999999999999756, 5.750000472440944144, 0.4108223460329293864 ) ) ;
#10656 = CARTESIAN_POINT ( 'NONE',  ( 3.507351867251836897, 2.016901088656855467, -0.6530382159986841684 ) ) ;
#10657 = CARTESIAN_POINT ( 'NONE',  ( 3.405153689607044232, 3.567999999999999616, -1.491010071662831171 ) ) ;
#10658 = AXIS2_PLACEMENT_3D ( 'NONE', #10930, #12990, #3899 ) ;
#10659 = LINE ( 'NONE', #12862, #13392 ) ;
#10660 = CONICAL_SURFACE ( 'NONE', #10903, 0.2944999999999998175, 0.7853981633974536081 ) ;
#10661 = EDGE_LOOP ( 'NONE', ( #5924, #12339, #4655, #9404 ) ) ;
#10662 = CARTESIAN_POINT ( 'NONE',  ( -0.4349147617188414694, 1.239999999999999991, -0.008611041693271251005 ) ) ;
#10663 = ORIENTED_EDGE ( 'NONE', *, *, #14653, .T. ) ;
#10664 = DIRECTION ( 'NONE',  ( -1.000000000000000000, -0.000000000000000000, -0.000000000000000000 ) ) ;
#10665 = ORIENTED_EDGE ( 'NONE', *, *, #9256, .F. ) ;
#10666 = MANIFOLD_SOLID_BREP ( 'Chamfer1', #13260 ) ;
#10667 = CARTESIAN_POINT ( 'NONE',  ( 1.130901178792395934, -0.4430000000000001714, -0.4240763015376258216 ) ) ;
#10668 = ADVANCED_FACE ( 'NONE', ( #10118 ), #1924, .T. ) ;
#10669 = AXIS2_PLACEMENT_3D ( 'NONE', #9063, #766, #6539 ) ;
#10670 = CYLINDRICAL_SURFACE ( 'NONE', #409, 0.03999999999999998002 ) ;
#10671 = EDGE_CURVE ( 'NONE', #799, #7678, #3897, .T. ) ;
#10672 = CARTESIAN_POINT ( 'NONE',  ( 0.6601485485260571995, -0.3723516483516483011, 0.5137583810202324131 ) ) ;
#10673 = VECTOR ( 'NONE', #14902, 39.37007874015748143 ) ;
#10674 = ORIENTED_EDGE ( 'NONE', *, *, #14111, .T. ) ;
#10675 = EDGE_LOOP ( 'NONE', ( #1538, #5077 ) ) ;
#10676 = ORIENTED_EDGE ( 'NONE', *, *, #12619, .F. ) ;
#10677 = B_SPLINE_CURVE_WITH_KNOTS ( 'NONE', 3,
 ( #13689, #7971, #14701, #6671, #8889, #7818 ),
 .UNSPECIFIED., .F., .F.,
 ( 4, 2, 4 ),
 ( 0.0008693723071205420889, 0.001360522261323142672, 0.001851672215525743256 ),
 .UNSPECIFIED. ) ;
#10678 = CARTESIAN_POINT ( 'NONE',  ( -0.3725000000000002198, 0.1859999999999983611, -0.4125000000000000333 ) ) ;
#10679 = CARTESIAN_POINT ( 'NONE',  ( 7.623651669702752511E-17, -0.6589999999999998082, 0.000000000000000000 ) ) ;
#10680 = AXIS2_PLACEMENT_3D ( 'NONE', #734, #14827, #3433 ) ;
#10681 = PLANE ( 'NONE',  #10062 ) ;
#10682 = CARTESIAN_POINT ( 'NONE',  ( 0.7072875780376989274, -0.01837860891257681734, -0.4734421766419254496 ) ) ;
#10683 = ORIENTED_EDGE ( 'NONE', *, *, #11951, .T. ) ;
#10684 = CARTESIAN_POINT ( 'NONE',  ( 3.694934205048947984, 1.926420985531493768, -0.4670271297431359270 ) ) ;
#10685 = CARTESIAN_POINT ( 'NONE',  ( 3.874999999999999556, 2.750000000000000000, -1.320000000000000062 ) ) ;
#10686 = DIRECTION ( 'NONE',  ( -1.000000000000000000, -0.000000000000000000, -0.000000000000000000 ) ) ;
#10687 = ADVANCED_FACE ( 'NONE', ( #9199 ), #5858, .T. ) ;
#10688 = ADVANCED_FACE ( 'NONE', ( #12853 ), #5752, .T. ) ;
#10689 = CIRCLE ( 'NONE', #3618, 1.749999999999999556 ) ;
#10690 = CARTESIAN_POINT ( 'NONE',  ( 1.398131049395801906, 0.007369456331666564795, -0.4802523863080122579 ) ) ;
#10691 = VERTEX_POINT ( 'NONE', #11410 ) ;
#10693 = ORIENTED_EDGE ( 'NONE', *, *, #14764, .F. ) ;
#10692 = FACE_OUTER_BOUND ( 'NONE', #1914, .T. ) ;
#10694 = ORIENTED_EDGE ( 'NONE', *, *, #10289, .F. ) ;
#10695 = FACE_OUTER_BOUND ( 'NONE', #4787, .T. ) ;
#10696 = ORIENTED_EDGE ( 'NONE', *, *, #10199, .F. ) ;
#10697 = CYLINDRICAL_SURFACE ( 'NONE', #14335, 0.3750000000000004996 ) ;
#10698 = CIRCLE ( 'NONE', #14875, 0.03999999999999998002 ) ;
#10699 = SHAPE_DEFINITION_REPRESENTATION ( #14213, #9930 ) ;
#10700 = CARTESIAN_POINT ( 'NONE',  ( 0.4124999999999999223, -0.6290000000000003366, 0.3724999999999999423 ) ) ;
#10701 = ORIENTED_EDGE ( 'NONE', *, *, #11663, .T. ) ;
#10702 = CARTESIAN_POINT ( 'NONE',  ( -0.1786439721334353026, 1.577722767886655886, -0.3809527529760087239 ) ) ;
#10703 = CYLINDRICAL_SURFACE ( 'NONE', #3157, 0.4349999999999999423 ) ;
#10704 = CIRCLE ( 'NONE', #7296, 0.7173254825712085392 ) ;
#10705 = CARTESIAN_POINT ( 'NONE',  ( 3.873439288382781065, 3.137999999999999901, 6.065921084684207584E-32 ) ) ;
#10706 = EDGE_CURVE ( 'NONE', #8264, #11613, #989, .T. ) ;
#10707 = DIRECTION ( 'NONE',  ( -1.874307916738608820E-16, 1.000000000000000000, 0.000000000000000000 ) ) ;
#10708 = CARTESIAN_POINT ( 'NONE',  ( 0.7017867892446607581, 0.04143956043956044388, -0.4010711782184314678 ) ) ;
#10709 = DIRECTION ( 'NONE',  ( -1.000000000000000000, -0.000000000000000000, -0.000000000000000000 ) ) ;
#10710 = CARTESIAN_POINT ( 'NONE',  ( 3.875000000000619504, 1.884022191776286714, 0.5000000000000002220 ) ) ;
#10711 = ORIENTED_EDGE ( 'NONE', *, *, #13123, .F. ) ;
#10712 = CARTESIAN_POINT ( 'NONE',  ( 0.6592591305498914922, -0.4437908075296089216, 0.4883895785410081736 ) ) ;
#10714 = ORIENTED_EDGE ( 'NONE', *, *, #8126, .T. ) ;
#10713 = CYLINDRICAL_SURFACE ( 'NONE', #11634, 0.3750000000000004996 ) ;
#10715 = CIRCLE ( 'NONE', #13634, 1.552690549202460968 ) ;
#10716 = EDGE_LOOP ( 'NONE', ( #6208, #14164, #7307, #7035 ) ) ;
#10717 = CIRCLE ( 'NONE', #2888, 1.000000000000000000 ) ;
#10718 = VECTOR ( 'NONE', #1053, 39.37007874015748143 ) ;
#10719 = CARTESIAN_POINT ( 'NONE',  ( -0.2099999999999999922, 0.7512260236060024354, -0.3809527529760087239 ) ) ;
#10720 =( NAMED_UNIT ( * ) PLANE_ANGLE_UNIT ( ) SI_UNIT ( $, .RADIAN. ) );
#10721 = CARTESIAN_POINT ( 'NONE',  ( 2.684185600478663503, 0.4127059874548060781, 0.4620877740044938009 ) ) ;
#10722 = ORIENTED_EDGE ( 'NONE', *, *, #3082, .F. ) ;
#10723 = VECTOR ( 'NONE', #4879, 39.37007874015748143 ) ;
#10724 = DIRECTION ( 'NONE',  ( 0.000000000000000000, 0.000000000000000000, -1.000000000000000000 ) ) ;
#10725 = CIRCLE ( 'NONE', #11191, 0.07000000000000047851 ) ;
#10726 = ADVANCED_FACE ( 'NONE', ( #67 ), #11224, .F. ) ;
#10727 = EDGE_CURVE ( 'NONE', #4509, #2057, #6591, .T. ) ;
#10728 = DIRECTION ( 'NONE',  ( 0.000000000000000000, 0.000000000000000000, 1.000000000000000000 ) ) ;
#10729 = ADVANCED_FACE ( 'NONE', ( #6753 ), #10339, .T. ) ;
#10730 = CIRCLE ( 'NONE', #4128, 1.000000000000000222 ) ;
#10731 = CIRCLE ( 'NONE', #4130, 2.500000000000000444 ) ;
#10732 = CYLINDRICAL_SURFACE ( 'NONE', #930, 1.749999999999999556 ) ;
#10733 = ORIENTED_EDGE ( 'NONE', *, *, #2231, .T. ) ;
#10734 = FACE_OUTER_BOUND ( 'NONE', #14684, .T. ) ;
#10735 = AXIS2_PLACEMENT_3D ( 'NONE', #1461, #5992, #5849 ) ;
#10736 = CARTESIAN_POINT ( 'NONE',  ( 0.06299999999999994493, 1.679378605318035733, -2.086378605318071511 ) ) ;
#10737 = CARTESIAN_POINT ( 'NONE',  ( 3.426491571325181340, 1.987932976489903414, 0.2209981660730357955 ) ) ;
#10738 = LINE ( 'NONE', #12316, #10481 ) ;
#10739 = ORIENTED_EDGE ( 'NONE', *, *, #11199, .F. ) ;
#10740 = ADVANCED_FACE ( 'NONE', ( #4454 ), #1066, .F. ) ;
#10741 = AXIS2_PLACEMENT_3D ( 'NONE', #7764, #13480, #12346 ) ;
#10742 = FACE_OUTER_BOUND ( 'NONE', #13439, .T. ) ;
#10743 = ORIENTED_EDGE ( 'NONE', *, *, #10338, .F. ) ;
#10744 = DIRECTION ( 'NONE',  ( 0.000000000000000000, 0.000000000000000000, -1.000000000000000000 ) ) ;
#10745 = ORIENTED_EDGE ( 'NONE', *, *, #8587, .F. ) ;
#10746 = DIRECTION ( 'NONE',  ( -0.000000000000000000, -1.000000000000000000, -0.000000000000000000 ) ) ;
#10747 = AXIS2_PLACEMENT_3D ( 'NONE', #13654, #15113, #11677 ) ;
#10748 = DIRECTION ( 'NONE',  ( 0.000000000000000000, 0.000000000000000000, -1.000000000000000000 ) ) ;
#10749 = EDGE_CURVE ( 'NONE', #710, #2919, #15139, .T. ) ;
#10750 = CIRCLE ( 'NONE', #1926, 0.7849999999999993650 ) ;
#10751 = DIRECTION ( 'NONE',  ( 2.602462600580851747E-17, 1.000000000000000000, -0.000000000000000000 ) ) ;
#10752 = DIRECTION ( 'NONE',  ( 0.000000000000000000, 0.000000000000000000, 1.000000000000000000 ) ) ;
#10753 = DIRECTION ( 'NONE',  ( -1.000000000000000000, -0.000000000000000000, -0.000000000000000000 ) ) ;
#10754 = VERTEX_POINT ( 'NONE', #2060 ) ;
#10755 = VERTEX_POINT ( 'NONE', #3045 ) ;
#10756 = VERTEX_POINT ( 'NONE', #4760 ) ;
#10757 = EDGE_CURVE ( 'NONE', #2639, #2008, #1936, .T. ) ;
#10758 = AXIS2_PLACEMENT_3D ( 'NONE', #3362, #4741, #1049 ) ;
#10759 = DIRECTION ( 'NONE',  ( -0.000000000000000000, -1.000000000000000000, -0.000000000000000000 ) ) ;
#10760 = DIRECTION ( 'NONE',  ( 8.659560562354900811E-17, -0.7071067811865501263, 0.7071067811865449082 ) ) ;
#10761 = DIRECTION ( 'NONE',  ( 0.000000000000000000, 0.000000000000000000, 1.000000000000000000 ) ) ;
#10762 = ADVANCED_FACE ( 'NONE', ( #3531 ), #3228, .T. ) ;
#10763 = CARTESIAN_POINT ( 'NONE',  ( 3.874999999999999556, 3.105999999999998984, -1.320000000000000062 ) ) ;
#10764 = ORIENTED_EDGE ( 'NONE', *, *, #7859, .T. ) ;
#10765 = DIRECTION ( 'NONE',  ( 0.000000000000000000, 0.000000000000000000, 1.000000000000000000 ) ) ;
#10766 = CARTESIAN_POINT ( 'NONE',  ( 3.426491571325181340, 0.9800000000000039790, 2.359999999999999876 ) ) ;
#10767 = ORIENTED_EDGE ( 'NONE', *, *, #11842, .T. ) ;
#10769 = ORIENTED_EDGE ( 'NONE', *, *, #10258, .F. ) ;
#10768 = CYLINDRICAL_SURFACE ( 'NONE', #3015, 0.7500000000000001110 ) ;
#10770 = ORIENTED_EDGE ( 'NONE', *, *, #11963, .F. ) ;
#10771 = CARTESIAN_POINT ( 'NONE',  ( 0.1949587543783453114, 1.569534359386387967, 0.3809527529760087239 ) ) ;
#10772 = ORIENTED_EDGE ( 'NONE', *, *, #4862, .F. ) ;
#10773 = ADVANCED_FACE ( 'NONE', ( #3457 ), #10503, .T. ) ;
#10774 = ADVANCED_FACE ( 'NONE', ( #4527 ), #7810, .F. ) ;
#10775 = EDGE_CURVE ( 'NONE', #4169, #14557, #14401, .T. ) ;
#10776 =( CONVERSION_BASED_UNIT ( 'INCH', #5115 ) LENGTH_UNIT ( ) NAMED_UNIT ( #482 ) );
#10777 = LINE ( 'NONE', #10700, #105 ) ;
#10778 = EDGE_LOOP ( 'NONE', ( #11694, #2926, #4543, #846 ) ) ;
#10779 = CARTESIAN_POINT ( 'NONE',  ( -0.2249147617188397563, 1.239999999999999991, 0.3723417112827376307 ) ) ;
#10780 = CARTESIAN_POINT ( 'NONE',  ( 2.774999999999999911, 1.575000000000016387, 2.359999999999999432 ) ) ;
#10781 = DIRECTION ( 'NONE',  ( 0.000000000000000000, 0.000000000000000000, 1.000000000000000000 ) ) ;
#10782 = DIRECTION ( 'NONE',  ( 1.000000000000000000, 0.000000000000000000, 0.000000000000000000 ) ) ;
#10783 = AXIS2_PLACEMENT_3D ( 'NONE', #12050, #11762, #1260 ) ;
#10784 = CYLINDRICAL_SURFACE ( 'NONE', #7968, 0.7849999999999996980 ) ;
#10785 = CARTESIAN_POINT ( 'NONE',  ( 6.208491571325183145, -1.679378605318048390, 1.304378605318053497 ) ) ;
#10786 = CARTESIAN_POINT ( 'NONE',  ( 0.8552050450108602542, -0.4750535095564970001, -0.4355134298035638341 ) ) ;
#10787 = CARTESIAN_POINT ( 'NONE',  ( 3.622127693352770184, 1.891608983934359500, 0.7060953400642342448 ) ) ;
#10788 = CARTESIAN_POINT ( 'NONE',  ( 3.874999999999999556, 3.567999999999999616, 1.320000000000000062 ) ) ;
#10789 = ORIENTED_EDGE ( 'NONE', *, *, #13411, .F. ) ;
#10790 = CARTESIAN_POINT ( 'NONE',  ( 5.567023771132172172, 0.000000000000000000, 1.580000000000000071 ) ) ;
#10792 = ORIENTED_EDGE ( 'NONE', *, *, #14654, .F. ) ;
#10791 = LINE ( 'NONE', #5907, #8234 ) ;
#10793 = ORIENTED_EDGE ( 'NONE', *, *, #1437, .T. ) ;
#10794 = DIRECTION ( 'NONE',  ( -0.2251194151855828718, -0.9743259920144011765, -0.003179652756857814528 ) ) ;
#10795 = EDGE_CURVE ( 'NONE', #10219, #4487, #9511, .T. ) ;
#10796 = CARTESIAN_POINT ( 'NONE',  ( 3.391025564058367525, 0.6913684120611767181, 0.4521041586997406325 ) ) ;
#10797 = ORIENTED_EDGE ( 'NONE', *, *, #725, .F. ) ;
#10798 = CIRCLE ( 'NONE', #13219, 0.4070000000000022489 ) ;
#10799 = CARTESIAN_POINT ( 'NONE',  ( 0.09500000000000431710, -1.679378605318048390, 2.054378605318054607 ) ) ;
#10800 = CARTESIAN_POINT ( 'NONE',  ( 0.7513246802501646338, 4.268512490100411279E-17, 0.4293820849162031661 ) ) ;
#10801 = DIRECTION ( 'NONE',  ( -0.7071067811865406894, 8.659560562355016675E-17, -0.7071067811865542341 ) ) ;
#10802 = ORIENTED_EDGE ( 'NONE', *, *, #6376, .F. ) ;
#10803 = CARTESIAN_POINT ( 'NONE',  ( -5.764454660286586870E-18, 0.1956296296296295978, 0.000000000000000000 ) ) ;
#10804 = VECTOR ( 'NONE', #4795, 39.37007874015748143 ) ;
#10805 = CYLINDRICAL_SURFACE ( 'NONE', #11798, 0.4850000000000000422 ) ;
#10806 = CARTESIAN_POINT ( 'NONE',  ( 8.789999999999999147, 0.9399413264884247665, 6.829619984160658046E-17 ) ) ;
#10807 = VERTEX_POINT ( 'NONE', #10271 ) ;
#10808 = DIRECTION ( 'NONE',  ( 0.000000000000000000, 1.000000000000000000, 0.000000000000000000 ) ) ;
#10809 = ORIENTED_EDGE ( 'NONE', *, *, #13155, .T. ) ;
#10810 = EDGE_CURVE ( 'NONE', #13120, #12826, #13017, .T. ) ;
#10811 = DIRECTION ( 'NONE',  ( 0.000000000000000000, 0.000000000000000000, -1.000000000000000000 ) ) ;
#10812 = VERTEX_POINT ( 'NONE', #12622 ) ;
#10813 = DIRECTION ( 'NONE',  ( 0.7071067811865436870, 8.659560562354978464E-17, 0.7071067811865512365 ) ) ;
#10814 = DIRECTION ( 'NONE',  ( 1.000000000000000000, -0.000000000000000000, -0.000000000000000000 ) ) ;
#10815 = DIRECTION ( 'NONE',  ( 0.000000000000000000, 0.000000000000000000, -1.000000000000000000 ) ) ;
#10816 = FACE_OUTER_BOUND ( 'NONE', #7321, .T. ) ;
#10817 = AXIS2_PLACEMENT_3D ( 'NONE', #11267, #11190, #10202 ) ;
#10818 = FILL_AREA_STYLE_COLOUR ( '', #1476 ) ;
#10819 = VERTEX_POINT ( 'NONE', #10799 ) ;
#10820 = ORIENTED_EDGE ( 'NONE', *, *, #6616, .T. ) ;
#10821 = ADVANCED_FACE ( 'NONE', ( #11869 ), #3640, .T. ) ;
#10822 = EDGE_LOOP ( 'NONE', ( #14411, #11776, #12910, #13767 ) ) ;
#10823 = ADVANCED_FACE ( 'NONE', ( #7361 ), #14160, .F. ) ;
#10824 = CARTESIAN_POINT ( 'NONE',  ( 8.477129920625907644, 0.8689790899078102537, -0.3802665265448318399 ) ) ;
#10825 = EDGE_CURVE ( 'NONE', #1772, #1104, #7291, .T. ) ;
#10826 = CARTESIAN_POINT ( 'NONE',  ( 2.774999999999999911, 2.360000000000015863, 0.9799999999999454703 ) ) ;
#10827 = DIRECTION ( 'NONE',  ( -1.000000000000000000, -0.000000000000000000, -0.000000000000000000 ) ) ;
#10828 = CARTESIAN_POINT ( 'NONE',  ( 3.426491571325181340, 0.9800000000000039790, 2.359999999999999876 ) ) ;
#10829 = LINE ( 'NONE', #8255, #6588 ) ;
#10830 = EDGE_CURVE ( 'NONE', #12064, #1986, #9567, .T. ) ;
#10831 = CARTESIAN_POINT ( 'NONE',  ( 0.000000000000000000, 0.000000000000000000, -0.2499999999999999167 ) ) ;
#10832 = CARTESIAN_POINT ( 'NONE',  ( 0.4349147617188408588, 1.559103846021540951, -0.008611041693278118775 ) ) ;
#10833 = AXIS2_PLACEMENT_3D ( 'NONE', #12322, #10116, #14771 ) ;
#10834 = CARTESIAN_POINT ( 'NONE',  ( 4.367450314957311619, 1.706859693599265926, -0.6280954649258110312 ) ) ;
#10835 = ORIENTED_EDGE ( 'NONE', *, *, #3172, .F. ) ;
#10837 = EDGE_LOOP ( 'NONE', ( #13866, #7755, #8000, #5131 ) ) ;
#10836 = CARTESIAN_POINT ( 'NONE',  ( 0.7034553201775799458, -0.4178655479186547117, -0.4790822413290380388 ) ) ;
#10838 = ORIENTED_EDGE ( 'NONE', *, *, #2991, .T. ) ;
#10839 = CARTESIAN_POINT ( 'NONE',  ( 0.8999999999999999112, -0.4829999999999998739, -0.3750000000000000555 ) ) ;
#10840 = CARTESIAN_POINT ( 'NONE',  ( 2.527624975756972425, 3.137999999999999901, 0.9199802545633498640 ) ) ;
#10841 = SHAPE_DEFINITION_REPRESENTATION ( #1628, #2091 ) ;
#10842 = CARTESIAN_POINT ( 'NONE',  ( 0.2849999999999999756, 5.750000000000000000, 0.4108223460329293864 ) ) ;
#10843 = ORIENTED_EDGE ( 'NONE', *, *, #3781, .F. ) ;
#10844 = AXIS2_PLACEMENT_3D ( 'NONE', #13299, #12168, #1681 ) ;
#10845 = LINE ( 'NONE', #6263, #2632 ) ;
#10846 = CARTESIAN_POINT ( 'NONE',  ( 2.807000000000000384, 1.679378605318059048, 1.679378605318041506 ) ) ;
#10847 = EDGE_CURVE ( 'NONE', #3733, #11243, #9727, .T. ) ;
#10848 =( GEOMETRIC_REPRESENTATION_CONTEXT ( 3 ) GLOBAL_UNCERTAINTY_ASSIGNED_CONTEXT ( ( #9074 ) ) GLOBAL_UNIT_ASSIGNED_CONTEXT ( ( #5199, #10720, #4916 ) ) REPRESENTATION_CONTEXT ( 'NONE', 'WORKASPACE' ) );
#10849 = DIRECTION ( 'NONE',  ( 0.000000000000000000, -0.7071067811865600072, 0.7071067811865350272 ) ) ;
#10850 = EDGE_CURVE ( 'NONE', #39, #15103, #1452, .T. ) ;
#10851 = DIRECTION ( 'NONE',  ( 0.000000000000000000, 0.000000000000000000, -1.000000000000000000 ) ) ;
#10852 = CARTESIAN_POINT ( 'NONE',  ( 0.8852267783403774404, -0.4626342325507599162, -0.4488287372993887692 ) ) ;
#10853 = EDGE_CURVE ( 'NONE', #8572, #498, #1410, .T. ) ;
#10854 = DIRECTION ( 'NONE',  ( 0.000000000000000000, 0.000000000000000000, 1.000000000000000000 ) ) ;
#10855 = AXIS2_PLACEMENT_3D ( 'NONE', #425, #497, #2747 ) ;
#10856 = CARTESIAN_POINT ( 'NONE',  ( 3.669034062028589283, 1.848124941201018112, 0.7795100282588544038 ) ) ;
#10858 = ORIENTED_EDGE ( 'NONE', *, *, #414, .T. ) ;
#10857 = FACE_OUTER_BOUND ( 'NONE', #14570, .T. ) ;
#10859 =( GEOMETRIC_REPRESENTATION_CONTEXT ( 3 ) GLOBAL_UNCERTAINTY_ASSIGNED_CONTEXT ( ( #11356 ) ) GLOBAL_UNIT_ASSIGNED_CONTEXT ( ( #10776, #7265, #7189 ) ) REPRESENTATION_CONTEXT ( 'NONE', 'WORKASPACE' ) );
#10860 = ORIENTED_EDGE ( 'NONE', *, *, #10910, .T. ) ;
#10861 = DIRECTION ( 'NONE',  ( 0.7071067811865436870, 8.659560562354978464E-17, 0.7071067811865512365 ) ) ;
#10863 = VERTEX_POINT ( 'NONE', #6286 ) ;
#10862 = DIRECTION ( 'NONE',  ( 1.000000000000000000, 0.000000000000000000, 0.000000000000000000 ) ) ;
#10864 = ORIENTED_EDGE ( 'NONE', *, *, #4647, .F. ) ;
#10865 = DIRECTION ( 'NONE',  ( 1.365923996832131609E-16, -1.000000000000000000, 0.000000000000000000 ) ) ;
#10866 =( NAMED_UNIT ( * ) SI_UNIT ( $, .STERADIAN. ) SOLID_ANGLE_UNIT ( ) );
#10867 = LINE ( 'NONE', #7721, #11101 ) ;
#10868 = ORIENTED_EDGE ( 'NONE', *, *, #156, .T. ) ;
#10869 = DIRECTION ( 'NONE',  ( 0.000000000000000000, -0.000000000000000000, -1.000000000000000000 ) ) ;
#10870 = CIRCLE ( 'NONE', #13042, 1.000000000000000222 ) ;
#10871 = DIMENSIONAL_EXPONENTS ( 1.000000000000000000, 0.000000000000000000, 0.000000000000000000, 0.000000000000000000, 0.000000000000000000, 0.000000000000000000, 0.000000000000000000 ) ;
#10872 = CONICAL_SURFACE ( 'NONE', #11855, 0.1899999999999996136, 0.7853981633974435050 ) ;
#10873 = CARTESIAN_POINT ( 'NONE',  ( 0.6940843099860303234, 0.04143956054457292176, 0.4145488311989756758 ) ) ;
#10874 = CARTESIAN_POINT ( 'NONE',  ( 6.794491571325181667, 1.679378605318059492, 1.679378605318041506 ) ) ;
#10875 = VERTEX_POINT ( 'NONE', #12015 ) ;
#10876 = EDGE_CURVE ( 'NONE', #4210, #15007, #420, .T. ) ;
#10877 = CARTESIAN_POINT ( 'NONE',  ( 0.4424999999999979505, -0.6589999999999996971, -0.8500000000000000888 ) ) ;
#10878 = DIRECTION ( 'NONE',  ( 0.000000000000000000, 0.000000000000000000, -1.000000000000000000 ) ) ;
#10879 = DIRECTION ( 'NONE',  ( -1.000000000000000000, -0.000000000000000000, -0.000000000000000000 ) ) ;
#10880 = ORIENTED_EDGE ( 'NONE', *, *, #4896, .T. ) ;
#10881 = CIRCLE ( 'NONE', #10146, 0.2944999999999998175 ) ;
#10882 = DIRECTION ( 'NONE',  ( 1.000000000000000000, 0.000000000000000000, 0.000000000000000000 ) ) ;
#10883 = EDGE_LOOP ( 'NONE', ( #4560, #6852, #9664, #5769 ) ) ;
#10884 = CIRCLE ( 'NONE', #8935, 1.494001693158433230 ) ;
#10885 = VECTOR ( 'NONE', #10331, 39.37007874015748143 ) ;
#10886 = CARTESIAN_POINT ( 'NONE',  ( 0.7371172985291578605, -0.0009284805720397705606, 0.4420151072446019125 ) ) ;
#10887 = ORIENTED_EDGE ( 'NONE', *, *, #532, .T. ) ;
#10888 = FACE_OUTER_BOUND ( 'NONE', #11608, .T. ) ;
#10889 = CARTESIAN_POINT ( 'NONE',  ( 0.9999999999999966693, -0.3829999999999998961, 0.4858757062146893402 ) ) ;
#10890 = CARTESIAN_POINT ( 'NONE',  ( 0.7830035894062601365, -0.4429999999999999494, -0.3557498141818015713 ) ) ;
#10891 = DIRECTION ( 'NONE',  ( 1.000000000000000000, 0.000000000000000000, 0.000000000000000000 ) ) ;
#10892 = VECTOR ( 'NONE', #9529, 39.37007874015748143 ) ;
#10893 = CIRCLE ( 'NONE', #3824, 0.2625000000000000111 ) ;
#10894 = CARTESIAN_POINT ( 'NONE',  ( 3.876560711617219379, -3.000039370078740220, -0.7500000000000001110 ) ) ;
#10895 = EDGE_CURVE ( 'NONE', #15105, #2972, #8044, .T. ) ;
#10896 = ORIENTED_EDGE ( 'NONE', *, *, #13329, .F. ) ;
#10897 = VERTEX_POINT ( 'NONE', #14303 ) ;
#10898 = ORIENTED_EDGE ( 'NONE', *, *, #8840, .T. ) ;
#10899 = CIRCLE ( 'NONE', #4306, 0.8000000000000000444 ) ;
#10900 = LINE ( 'NONE', #5092, #12353 ) ;
#10901 = DIRECTION ( 'NONE',  ( 0.000000000000000000, 0.000000000000000000, -1.000000000000000000 ) ) ;
#10902 = AXIS2_PLACEMENT_3D ( 'NONE', #15066, #1211, #13827 ) ;
#10903 = AXIS2_PLACEMENT_3D ( 'NONE', #1623, #6313, #2079 ) ;
#10904 = CARTESIAN_POINT ( 'NONE',  ( 3.874999999999999556, 3.567999999999999616, 1.097499999999999920 ) ) ;
#10905 = CARTESIAN_POINT ( 'NONE',  ( 0.000000000000000000, 1.000000000000000000, -0.6614378277661475680 ) ) ;
#10906 = DIRECTION ( 'NONE',  ( 0.000000000000000000, 0.000000000000000000, 1.000000000000000000 ) ) ;
#10907 = CARTESIAN_POINT ( 'NONE',  ( 4.485106214549655412, 1.787785851493574274, -0.4390631173008620047 ) ) ;
#10908 = ADVANCED_FACE ( 'NONE', ( #3917 ), #2155, .F. ) ;
#10909 = B_SPLINE_CURVE_WITH_KNOTS ( 'NONE', 3,
 ( #5198, #13362, #10941, #11011, #9724, #12300, #5271, #2905, #9793, #6425, #13512, #11078, #576, #9943, #5061, #12011 ),
 .UNSPECIFIED., .F., .F.,
 ( 4, 2, 2, 2, 2, 2, 2, 4 ),
 ( 0.000000000000000000, 0.0005886476847306626632, 0.001177295369461325326, 0.001765943054191987990, 0.002354590738922650653, 0.002943238423653313316, 0.003531886108383975979, 0.004709181477845301306 ),
 .UNSPECIFIED. ) ;
#10910 = EDGE_CURVE ( 'NONE', #13774, #3778, #288, .T. ) ;
#10911 = AXIS2_PLACEMENT_3D ( 'NONE', #14824, #7715, #3352 ) ;
#10912 = SHAPE_REPRESENTATION ( 'Outlet Housing', ( #8424 ), #7206 ) ;
#10913 = ADVANCED_FACE ( 'NONE', ( #4991 ), #12083, .T. ) ;
#10914 = AXIS2_PLACEMENT_3D ( 'NONE', #8411, #4897, #4814 ) ;
#10915 = ORIENTED_EDGE ( 'NONE', *, *, #8595, .F. ) ;
#10916 = ORIENTED_EDGE ( 'NONE', *, *, #10412, .T. ) ;
#10917 = EDGE_CURVE ( 'NONE', #8716, #7260, #7776, .T. ) ;
#10918 = ORIENTED_EDGE ( 'NONE', *, *, #8216, .F. ) ;
#10919 = DIRECTION ( 'NONE',  ( -1.365923996832131609E-16, 1.000000000000000000, 0.000000000000000000 ) ) ;
#10920 = CARTESIAN_POINT ( 'NONE',  ( 1.250847373107698779, -0.05999999999999997696, -0.4823326642216426707 ) ) ;
#10921 = DIRECTION ( 'NONE',  ( 0.000000000000000000, 0.000000000000000000, 1.000000000000000000 ) ) ;
#10922 = CONICAL_SURFACE ( 'NONE', #13341, 0.05500000000000146438, 0.7853981633974547183 ) ;
#10923 = PRODUCT_CONTEXT ( 'NONE', #7067, 'mechanical' ) ;
#10924 = CARTESIAN_POINT ( 'NONE',  ( 2.418884559267909129, 0.5995087936327320177, 0.4658349638521481761 ) ) ;
#10925 = EDGE_LOOP ( 'NONE', ( #6999, #4022, #2950, #767 ) ) ;
#10926 = DIRECTION ( 'NONE',  ( 0.01412288512831128343, 0.000000000000000000, 0.9999002670844990837 ) ) ;
#10927 = DIRECTION ( 'NONE',  ( -0.9999002670844991947, -1.365787769249574922E-16, 0.01412288512831213171 ) ) ;
#10928 = CARTESIAN_POINT ( 'NONE',  ( 3.492055192262802699, 2.024943995107577166, 0.6451593962764085033 ) ) ;
#10929 = AXIS2_PLACEMENT_3D ( 'NONE', #8848, #2098, #4336 ) ;
#10930 = CARTESIAN_POINT ( 'NONE',  ( -0.3724999999999999423, 0.1749999999999999889, -0.3724999999999999978 ) ) ;
#10931 = DIRECTION ( 'NONE',  ( -0.3420201433256628287, 0.000000000000000000, -0.9396926207859105373 ) ) ;
#10932 = CARTESIAN_POINT ( 'NONE',  ( 3.790134320942320389, 1.827873989719922321, 0.7454134881782992217 ) ) ;
#10933 = CYLINDRICAL_SURFACE ( 'NONE', #10855, 0.2625000000000000111 ) ;
#10934 = ORIENTED_EDGE ( 'NONE', *, *, #3534, .F. ) ;
#10935 = CARTESIAN_POINT ( 'NONE',  ( 0.000000000000000000, 0.000000000000000000, 1.500000000000000222 ) ) ;
#10937 = ORIENTED_EDGE ( 'NONE', *, *, #10137, .F. ) ;
#10936 = CARTESIAN_POINT ( 'NONE',  ( 2.599160627732594264, 0.7974701832127792933, -0.4632886916986921344 ) ) ;
#10938 = VERTEX_POINT ( 'NONE', #11796 ) ;
#10939 = VECTOR ( 'NONE', #4510, 39.37007874015748854 ) ;
#10940 = ADVANCED_FACE ( 'NONE', ( #361 ), #5065, .F. ) ;
#10941 = CARTESIAN_POINT ( 'NONE',  ( 0.6570999327328048700, -0.05543034563825118000, 0.5130307608016103638 ) ) ;
#10942 = DIRECTION ( 'NONE',  ( 0.000000000000000000, 0.000000000000000000, -1.000000000000000000 ) ) ;
#10943 = ORIENTED_EDGE ( 'NONE', *, *, #9137, .F. ) ;
#10944 = DIRECTION ( 'NONE',  ( 0.000000000000000000, 0.000000000000000000, 1.000000000000000000 ) ) ;
#10945 = EDGE_CURVE ( 'NONE', #12302, #2942, #14127, .T. ) ;
#10946 = CARTESIAN_POINT ( 'NONE',  ( 0.6735393331370996828, 0.02844630743745005588, 0.4543474816912275727 ) ) ;
#10947 = DIRECTION ( 'NONE',  ( -0.000000000000000000, -1.000000000000000000, -0.000000000000000000 ) ) ;
#10948 = TOROIDAL_SURFACE ( 'NONE', #169, 1.552690549202460968, 0.05999999999999999778 ) ;
#10949 = EDGE_LOOP ( 'NONE', ( #10399, #3929, #4173, #13533, #7866 ) ) ;
#10950 = DIRECTION ( 'NONE',  ( 1.000000000000000000, 0.000000000000000000, 0.000000000000000000 ) ) ;
#10951 = LINE ( 'NONE', #5147, #5104 ) ;
#10952 = CARTESIAN_POINT ( 'NONE',  ( 0.8999999999999998002, 0.1749999999999999889, -0.3799999999999999489 ) ) ;
#10953 = VECTOR ( 'NONE', #6664, 39.37007874015748854 ) ;
#10954 = DIRECTION ( 'NONE',  ( 0.000000000000000000, 0.000000000000000000, -1.000000000000000000 ) ) ;
#10955 = EDGE_LOOP ( 'NONE', ( #4602, #14124, #5478, #5174 ) ) ;
#10956 = AXIS2_PLACEMENT_3D ( 'NONE', #9313, #9546, #12808 ) ;
#10957 = CARTESIAN_POINT ( 'NONE',  ( 3.874999999999999556, 3.137999999999999901, -1.320000000000000062 ) ) ;
#10958 = EDGE_LOOP ( 'NONE', ( #11679, #2437 ) ) ;
#10959 = AXIS2_PLACEMENT_3D ( 'NONE', #12602, #11545, #15062 ) ;
#10960 = DIRECTION ( 'NONE',  ( 1.000000000000000000, -0.000000000000000000, -0.000000000000000000 ) ) ;
#10961 =( REPRESENTATION_RELATIONSHIP ('NONE','NONE', #3591, #2091 ) REPRESENTATION_RELATIONSHIP_WITH_TRANSFORMATION ( #13491 )SHAPE_REPRESENTATION_RELATIONSHIP( ) );
#10962 = VERTEX_POINT ( 'NONE', #8295 ) ;
#10963 = ADVANCED_FACE ( 'NONE', ( #8875 ), #4213, .F. ) ;
#10964 = EDGE_CURVE ( 'NONE', #10623, #9809, #6430, .T. ) ;
#10965 = AXIS2_PLACEMENT_3D ( 'NONE', #14247, #10891, #10752 ) ;
#10966 = DIRECTION ( 'NONE',  ( -0.000000000000000000, 1.000000000000000000, -0.000000000000000000 ) ) ;
#10967 = AXIS2_PLACEMENT_3D ( 'NONE', #12763, #4675, #9422 ) ;
#10968 = DIRECTION ( 'NONE',  ( 0.7070715176384831935, 0.7070715176384805289, -0.009986885842351453380 ) ) ;
#10969=STYLED_ITEM('',(#15185),#10334);
#10970 = CIRCLE ( 'NONE', #4380, 0.2944999999999998175 ) ;
#10971 = AXIS2_PLACEMENT_3D ( 'NONE', #2869, #7686, #14721 ) ;
#10972 = CYLINDRICAL_SURFACE ( 'NONE', #8914, 0.1899999999999996136 ) ;
#10973 = FACE_OUTER_BOUND ( 'NONE', #6672, .T. ) ;
#10974 = ORIENTED_EDGE ( 'NONE', *, *, #10363, .F. ) ;
#10975 = VERTEX_POINT ( 'NONE', #5435 ) ;
#10976 = VERTEX_POINT ( 'NONE', #9950 ) ;
#10977 = DIRECTION ( 'NONE',  ( -1.000000000000000000, -0.000000000000000000, -0.000000000000000000 ) ) ;
#10978 = LINE ( 'NONE', #7392, #5804 ) ;
#10979 = CARTESIAN_POINT ( 'NONE',  ( 2.774999999999999911, 1.679378605318059048, 1.679378605318041506 ) ) ;
#10980 = CARTESIAN_POINT ( 'NONE',  ( 0.9749999999999999778, -0.6429999999999999050, -0.3750000000000000555 ) ) ;
#10981 = DIRECTION ( 'NONE',  ( 1.000000000000000000, 0.000000000000000000, 0.000000000000000000 ) ) ;
#10982 = CARTESIAN_POINT ( 'NONE',  ( 4.625398766514281945, 1.810313843597131100, -0.04860614483416566406 ) ) ;
#10983 = B_SPLINE_CURVE_WITH_KNOTS ( 'NONE', 3,
 ( #6545, #6319, #11122, #2868, #7463, #7684, #5318, #5097, #7396, #14419, #13186, #12343 ),
 .UNSPECIFIED., .F., .F.,
 ( 4, 2, 2, 2, 2, 4 ),
 ( 4.252726876253797924E-17, 0.0004594653927451592497, 0.0009189307854902759986, 0.001837861570980509496, 0.002756792356470742777, 0.003675723141960976492 ),
 .UNSPECIFIED. ) ;
#10984 = FACE_OUTER_BOUND ( 'NONE', #1689, .T. ) ;
#10985 = VECTOR ( 'NONE', #10813, 39.37007874015748854 ) ;
#10986 = CARTESIAN_POINT ( 'NONE',  ( 4.285697740953402501, 1.709640378115386383, -0.6816790960877695538 ) ) ;
#10987 = ORIENTED_EDGE ( 'NONE', *, *, #10170, .T. ) ;
#10988 = ORIENTED_EDGE ( 'NONE', *, *, #9901, .T. ) ;
#10989 = EDGE_LOOP ( 'NONE', ( #6498, #2717, #9882, #9767 ) ) ;
#10990 = CARTESIAN_POINT ( 'NONE',  ( 0.2028461515626820422, 1.564725569476186795, 0.3809527529760088904 ) ) ;
#10991 = ADVANCED_FACE ( 'NONE', ( #1674 ), #4055, .F. ) ;
#10992 = DIRECTION ( 'NONE',  ( 0.000000000000000000, 0.000000000000000000, -1.000000000000000000 ) ) ;
#10993 = DIRECTION ( 'NONE',  ( -0.4999999999999998335, 0.000000000000000000, -0.8660254037844385966 ) ) ;
#10994 = CARTESIAN_POINT ( 'NONE',  ( 3.426491571325181340, 1.574999999999994849, -1.575000000000022160 ) ) ;
#10995 = ORIENTED_EDGE ( 'NONE', *, *, #3381, .T. ) ;
#10996 = LINE ( 'NONE', #6188, #8993 ) ;
#10997 = LINE ( 'NONE', #719, #4877 ) ;
#10998 = DIRECTION ( 'NONE',  ( -1.365923996832131609E-16, 1.000000000000000000, 0.000000000000000000 ) ) ;
#10999 = EDGE_CURVE ( 'NONE', #8264, #11902, #2892, .T. ) ;
#11000 = DIRECTION ( 'NONE',  ( 1.000000000000000000, 0.000000000000000000, 0.000000000000000000 ) ) ;
#11001 = CARTESIAN_POINT ( 'NONE',  ( 0.8444447451257305337, -0.4472863611497946423, -0.4262169690687090395 ) ) ;
#11002 = CARTESIAN_POINT ( 'NONE',  ( 6.787121492585022509, 1.224646799147353207E-16, 1.000000000000000000 ) ) ;
#11004 = VERTEX_POINT ( 'NONE', #5277 ) ;
#11003 = FACE_BOUND ( 'NONE', #12430, .T. ) ;
#11005 = VERTEX_POINT ( 'NONE', #662 ) ;
#11006 = CARTESIAN_POINT ( 'NONE',  ( 3.874999999999999556, 2.750000000000000000, -1.542000000000000037 ) ) ;
#11008 = VERTEX_POINT ( 'NONE', #8803 ) ;
#11007 = DIRECTION ( 'NONE',  ( -1.000000000000000000, -0.000000000000000000, -0.000000000000000000 ) ) ;
#11009 = ORIENTED_EDGE ( 'NONE', *, *, #822, .T. ) ;
#11010 = EDGE_CURVE ( 'NONE', #9310, #5214, #7066, .T. ) ;
#11011 = CARTESIAN_POINT ( 'NONE',  ( 0.6555297760382670091, -0.04033343379914773597, 0.5099209754895145386 ) ) ;
#11012 = CARTESIAN_POINT ( 'NONE',  ( -0.2249147617188397563, 0.7512260236060024354, 0.3723417112827376307 ) ) ;
#11013 = ORIENTED_EDGE ( 'NONE', *, *, #9186, .T. ) ;
#11014 = EDGE_CURVE ( 'NONE', #799, #9252, #14756, .T. ) ;
#11015 = CARTESIAN_POINT ( 'NONE',  ( -0.4125000000000000333, -0.6590000000000000302, 0.3724999999999999423 ) ) ;
#11016 = DIRECTION ( 'NONE',  ( -1.000000000000000000, -0.000000000000000000, -0.000000000000000000 ) ) ;
#11017 =( GEOMETRIC_REPRESENTATION_CONTEXT ( 3 ) GLOBAL_UNCERTAINTY_ASSIGNED_CONTEXT ( ( #5556 ) ) GLOBAL_UNIT_ASSIGNED_CONTEXT ( ( #1489, #1560, #5101 ) ) REPRESENTATION_CONTEXT ( 'NONE', 'WORKASPACE' ) );
#11018 = EDGE_CURVE ( 'NONE', #6943, #5889, #5362, .T. ) ;
#11019 = CARTESIAN_POINT ( 'NONE',  ( 0.7017867892446607581, 0.04143956043956047164, 0.4010711782184315233 ) ) ;
#11020 = DIRECTION ( 'NONE',  ( 0.000000000000000000, 0.000000000000000000, 1.000000000000000000 ) ) ;
#11021 = EDGE_CURVE ( 'NONE', #12552, #10819, #14451, .T. ) ;
#11022 = ORIENTED_EDGE ( 'NONE', *, *, #8245, .F. ) ;
#11023 = DIRECTION ( 'NONE',  ( 8.659560562354914369E-17, 0.7071067811865490160, -0.7071067811865459074 ) ) ;
#11024 = CARTESIAN_POINT ( 'NONE',  ( 3.875000000000000000, 3.535499999999999865, 0.000000000000000000 ) ) ;
#11025 = DIRECTION ( 'NONE',  ( 0.000000000000000000, 0.000000000000000000, 1.000000000000000000 ) ) ;
#11026 = FACE_OUTER_BOUND ( 'NONE', #9297, .T. ) ;
#11027 = ORIENTED_EDGE ( 'NONE', *, *, #14562, .F. ) ;
#11028 = CARTESIAN_POINT ( 'NONE',  ( -0.2578780456881166749, 1.589927591219160385, 0.3152476286636298197 ) ) ;
#11029 = ORIENTED_EDGE ( 'NONE', *, *, #12956, .F. ) ;
#11030 = DIRECTION ( 'NONE',  ( -0.000000000000000000, -1.000000000000000000, -0.000000000000000000 ) ) ;
#11031 = DIRECTION ( 'NONE',  ( -1.000000000000000000, -0.000000000000000000, -0.000000000000000000 ) ) ;
#11032 = EDGE_CURVE ( 'NONE', #754, #7123, #921, .T. ) ;
#11033 = DIRECTION ( 'NONE',  ( 1.000000000000000000, 0.000000000000000000, 0.000000000000000000 ) ) ;
#11034 = CIRCLE ( 'NONE', #4211, 1.812000000000000277 ) ;
#11035 = DIRECTION ( 'NONE',  ( 0.7071067811865497932, -0.7071067811865452413, 0.000000000000000000 ) ) ;
#11036 = DIRECTION ( 'NONE',  ( 0.4999999999999998335, 0.000000000000000000, 0.8660254037844388186 ) ) ;
#11037 = DIRECTION ( 'NONE',  ( -0.7071067811865429098, 0.000000000000000000, 0.7071067811865521247 ) ) ;
#11038 = ADVANCED_FACE ( 'NONE', ( #1741 ), #10465, .F. ) ;
#11039 = ORIENTED_EDGE ( 'NONE', *, *, #14661, .T. ) ;
#11040 = EDGE_LOOP ( 'NONE', ( #1737, #3806, #3885, #2274 ) ) ;
#11041 = ORIENTED_EDGE ( 'NONE', *, *, #13034, .F. ) ;
#11042 = CARTESIAN_POINT ( 'NONE',  ( 8.840371647876699157, 0.8816637705349000820, -0.09817148304380067525 ) ) ;
#11043 = ORIENTED_EDGE ( 'NONE', *, *, #2533, .T. ) ;
#11044 = DIRECTION ( 'NONE',  ( 0.000000000000000000, -0.7071067811865421326, -0.7071067811865530128 ) ) ;
#11045 = DIRECTION ( 'NONE',  ( -0.000000000000000000, 1.000000000000000000, -0.000000000000000000 ) ) ;
#11046 = DIRECTION ( 'NONE',  ( -1.000000000000000000, 0.000000000000000000, 0.000000000000000000 ) ) ;
#11047 = CARTESIAN_POINT ( 'NONE',  ( 3.876560711617219379, 1.855806856933289950, 0.7500000000000001110 ) ) ;
#11048 = VECTOR ( 'NONE', #7734, 39.37007874015748854 ) ;
#11049 = CARTESIAN_POINT ( 'NONE',  ( 2.414633059664291093, 0.1432059349181007413, 0.4658950132815778411 ) ) ;
#11050 = EDGE_CURVE ( 'NONE', #13629, #9095, #13860, .T. ) ;
#11051 = CARTESIAN_POINT ( 'NONE',  ( 4.161191225369840652, 1.720662318184893680, -0.7422136750874308575 ) ) ;
#11052 = ORIENTED_EDGE ( 'NONE', *, *, #1676, .T. ) ;
#11053 = EDGE_LOOP ( 'NONE', ( #4653, #13443, #10073, #9973 ) ) ;
#11054 = ORIENTED_EDGE ( 'NONE', *, *, #13600, .T. ) ;
#11055 = DIRECTION ( 'NONE',  ( -1.365923996832131609E-16, 1.000000000000000000, 0.000000000000000000 ) ) ;
#11056 = DIMENSIONAL_EXPONENTS ( 1.000000000000000000, 0.000000000000000000, 0.000000000000000000, 0.000000000000000000, 0.000000000000000000, 0.000000000000000000, 0.000000000000000000 ) ;
#11057 = CIRCLE ( 'NONE', #14723, 0.5000000000000002220 ) ;
#11058 = DIRECTION ( 'NONE',  ( 0.000000000000000000, 1.000000000000000000, 0.000000000000000000 ) ) ;
#11059 = CARTESIAN_POINT ( 'NONE',  ( 4.368421302294625441, 0.9967228440525767175, -0.08252939445393610296 ) ) ;
#11060 = CONTEXT_DEPENDENT_SHAPE_REPRESENTATION ( #2354, #9711 ) ;
#11061 = CARTESIAN_POINT ( 'NONE',  ( 3.348322488999904145, 0.9844945895124916913, 0.4527073094774024531 ) ) ;
#11062 = ORIENTED_EDGE ( 'NONE', *, *, #1110, .T. ) ;
#11063 = CARTESIAN_POINT ( 'NONE',  ( 2.633946444925666874, 0.3625193201794746356, -0.4033906250602100618 ) ) ;
#11064 = CARTESIAN_POINT ( 'NONE',  ( 2.124999999999999556, -2.360000000000016751, -0.9799999999999431388 ) ) ;
#11065 = CARTESIAN_POINT ( 'NONE',  ( 3.426491571325181340, 0.000000000000000000, 0.000000000000000000 ) ) ;
#11066 = AXIS2_PLACEMENT_3D ( 'NONE', #14639, #2582, #762 ) ;
#11067 = DIRECTION ( 'NONE',  ( 0.8841960195243572240, 0.000000000000000000, 0.4671160445299247232 ) ) ;
#11068 = CARTESIAN_POINT ( 'NONE',  ( 0.9317123296983564895, -0.4679219388635364463, -0.4432830823677768595 ) ) ;
#11069 = CARTESIAN_POINT ( 'NONE',  ( 4.307438648313010710, 1.779872554500928628, 0.6141414098449724523 ) ) ;
#11071 = ORIENTED_EDGE ( 'NONE', *, *, #9536, .F. ) ;
#11070 = LINE ( 'NONE', #14589, #5485 ) ;
#11072 = EDGE_LOOP ( 'NONE', ( #673, #8203, #10512, #8312 ) ) ;
#11073 = CONICAL_SURFACE ( 'NONE', #14990, 0.3750000000000004996, 0.7853981633974514986 ) ;
#11075 = ORIENTED_EDGE ( 'NONE', *, *, #2248, .F. ) ;
#11074 = FACE_OUTER_BOUND ( 'NONE', #11248, .T. ) ;
#11076 = ORIENTED_EDGE ( 'NONE', *, *, #7740, .T. ) ;
#11077 = AXIS2_PLACEMENT_3D ( 'NONE', #6444, #1913, #6600 ) ;
#11078 = CARTESIAN_POINT ( 'NONE',  ( 0.6735138268600963096, 0.02841772179894979516, 0.4544009417003765927 ) ) ;
#11079 = DIRECTION ( 'NONE',  ( -0.000000000000000000, -1.000000000000000000, -0.000000000000000000 ) ) ;
#11080 =( BOUNDED_CURVE ( )  B_SPLINE_CURVE ( 3, ( #7249, #5871, #10451, #4717 ),
 .UNSPECIFIED., .F., .F. ) 
 B_SPLINE_CURVE_WITH_KNOTS ( ( 4, 4 ),
 ( 4.712388980384689674, 5.497787143782132624 ),
 .UNSPECIFIED. ) 
 CURVE ( )  GEOMETRIC_REPRESENTATION_ITEM ( )  RATIONAL_B_SPLINE_CURVE ( ( 1.000000000000000000, 0.9492530216741918991, 0.9492530216741918991, 1.000000000000000000 ) ) 
 REPRESENTATION_ITEM ( '' )  );
#11081 = VERTEX_POINT ( 'NONE', #9797 ) ;
#11082 = DIRECTION ( 'NONE',  ( 0.000000000000000000, 0.000000000000000000, -1.000000000000000000 ) ) ;
#11083 = DIRECTION ( 'NONE',  ( 0.000000000000000000, 0.000000000000000000, -1.000000000000000000 ) ) ;
#11084 = CARTESIAN_POINT ( 'NONE',  ( 0.09035531712817648775, 1.379999999999999671, -0.1564999999999998892 ) ) ;
#11085 = CARTESIAN_POINT ( 'NONE',  ( 2.124999999999999556, 2.296212748401287479E-16, 1.875000000000000000 ) ) ;
#11086 = CIRCLE ( 'NONE', #14758, 1.124999999999998446 ) ;
#11087 = EDGE_CURVE ( 'NONE', #7417, #14371, #3056, .T. ) ;
#11088 = CARTESIAN_POINT ( 'NONE',  ( 0.06299999999999994493, -1.679378605318048390, 2.086378605318059964 ) ) ;
#11089 = AXIS2_PLACEMENT_3D ( 'NONE', #8032, #13741, #12681 ) ;
#11090 = EDGE_CURVE ( 'NONE', #14804, #3133, #10725, .T. ) ;
#11091 = ORIENTED_EDGE ( 'NONE', *, *, #12261, .F. ) ;
#11092 = ADVANCED_FACE ( 'NONE', ( #1896 ), #13595, .F. ) ;
#11093 = CARTESIAN_POINT ( 'NONE',  ( 8.469665986256828205, 0.8689060174719044349, 6.829619984160658046E-17 ) ) ;
#11094 = CARTESIAN_POINT ( 'NONE',  ( 3.875000000000000000, 3.567999999999999616, -0.5175000000000000711 ) ) ;
#11095 = DIRECTION ( 'NONE',  ( -1.000000000000000000, -0.000000000000000000, -0.000000000000000000 ) ) ;
#11096 = ORIENTED_EDGE ( 'NONE', *, *, #9336, .T. ) ;
#11097 = CARTESIAN_POINT ( 'NONE',  ( 4.098045170698160433, 0.8941794442107894314, -0.4477920867524256554 ) ) ;
#11098 = LINE ( 'NONE', #12319, #4790 ) ;
#11099 = ORIENTED_EDGE ( 'NONE', *, *, #2305, .F. ) ;
#11100 = EDGE_CURVE ( 'NONE', #1733, #1986, #6559, .T. ) ;
#11101 = VECTOR ( 'NONE', #8718, 39.37007874015748854 ) ;
#11102 = LINE ( 'NONE', #1987, #2779 ) ;
#11103 = ORIENTED_EDGE ( 'NONE', *, *, #9606, .T. ) ;
#11104 = FILL_AREA_STYLE ('',( #1758 ) ) ;
#11105 = CARTESIAN_POINT ( 'NONE',  ( 6.826491571325181695, -1.679378605318047946, -1.272378605318051248 ) ) ;
#11106 = CARTESIAN_POINT ( 'NONE',  ( 0.8418300605894719624, -0.4829999999999998739, -0.3276580719765713190 ) ) ;
#11107 = DIRECTION ( 'NONE',  ( 0.000000000000000000, 0.000000000000000000, 1.000000000000000000 ) ) ;
#11108 = AXIS2_PLACEMENT_3D ( 'NONE', #5959, #12750, #4817 ) ;
#11109 = CARTESIAN_POINT ( 'NONE',  ( 3.876560711617219379, -3.000039370078740220, 0.7500000000000001110 ) ) ;
#11110 = CARTESIAN_POINT ( 'NONE',  ( 1.542522555076166313, 0.03620193991704893921, -0.4782129582615927132 ) ) ;
#11111 = CONICAL_SURFACE ( 'NONE', #4275, 0.1899999999999996136, 0.7853981633974530530 ) ;
#11112 = DIRECTION ( 'NONE',  ( -1.000000000000000000, -0.000000000000000000, -0.000000000000000000 ) ) ;
#11113 = VERTEX_POINT ( 'NONE', #12234 ) ;
#11114 = ORIENTED_EDGE ( 'NONE', *, *, #602, .T. ) ;
#11115 = ORIENTED_EDGE ( 'NONE', *, *, #7488, .T. ) ;
#11116 = CARTESIAN_POINT ( 'NONE',  ( 8.783907589752294243, 0.8796920021765863851, -0.08309344507350861775 ) ) ;
#11117 = VERTEX_POINT ( 'NONE', #2983 ) ;
#11118 = DIRECTION ( 'NONE',  ( 0.000000000000000000, 1.000000000000000000, 0.000000000000000000 ) ) ;
#11119 = ADVANCED_FACE ( 'NONE', ( #3139 ), #8761, .F. ) ;
#11120 = LINE ( 'NONE', #14646, #12488 ) ;
#11121 = CIRCLE ( 'NONE', #9179, 2.960629921259842146 ) ;
#11122 = CARTESIAN_POINT ( 'NONE',  ( 3.426491571325181784, 2.050035007886724436, -0.6006740390345088887 ) ) ;
#11123 = AXIS2_PLACEMENT_3D ( 'NONE', #5202, #13365, #14519 ) ;
#11124 = CIRCLE ( 'NONE', #6490, 1.500000000000000222 ) ;
#11125 = EDGE_CURVE ( 'NONE', #733, #7670, #6087, .T. ) ;
#11126 = CARTESIAN_POINT ( 'NONE',  ( 4.470399241404178881, 1.786230780441887545, -0.4587633099568068085 ) ) ;
#11127 = VERTEX_POINT ( 'NONE', #6813 ) ;
#11128 = CARTESIAN_POINT ( 'NONE',  ( -0.2249147617188422543, 1.239999999999999991, -0.3723417112827361319 ) ) ;
#11129 = CONICAL_SURFACE ( 'NONE', #2347, 3.000000000000000444, 0.7853981633974568277 ) ;
#11130 = ORIENTED_EDGE ( 'NONE', *, *, #10260, .T. ) ;
#11131 = CIRCLE ( 'NONE', #608, 0.06000000000000004635 ) ;
#11132 = VERTEX_POINT ( 'NONE', #2208 ) ;
#11133 = ORIENTED_EDGE ( 'NONE', *, *, #9379, .F. ) ;
#11134 = DIRECTION ( 'NONE',  ( -0.9999002670844989726, 2.602203049398213494E-17, -0.01412288512831212997 ) ) ;
#11135 = CYLINDRICAL_SURFACE ( 'NONE', #11899, 1.000000000000000000 ) ;
#11136 = DIRECTION ( 'NONE',  ( 0.000000000000000000, -0.000000000000000000, 1.000000000000000000 ) ) ;
#11137 = CONTEXT_DEPENDENT_SHAPE_REPRESENTATION ( #5007, #522 ) ;
#11138 = CARTESIAN_POINT ( 'NONE',  ( 3.340400805683176877, 1.044207302812038440, 0.4528191976597221169 ) ) ;
#11139 = ORIENTED_EDGE ( 'NONE', *, *, #7230, .F. ) ;
#11140 = CARTESIAN_POINT ( 'NONE',  ( 3.394491571325183088, -1.679378605318041950, 1.679378605318059048 ) ) ;
#11141 = CYLINDRICAL_SURFACE ( 'NONE', #2913, 0.06000000000000001860 ) ;
#11142 = EDGE_CURVE ( 'NONE', #7890, #14925, #891, .T. ) ;
#11143 = ADVANCED_FACE ( 'NONE', ( #1127 ), #4666, .F. ) ;
#11144 = CIRCLE ( 'NONE', #7731, 1.552690549202460968 ) ;
#11145 = LINE ( 'NONE', #5184, #8739 ) ;
#11146 = CYLINDRICAL_SURFACE ( 'NONE', #1353, 0.7500000000000001110 ) ;
#11147 = CARTESIAN_POINT ( 'NONE',  ( 4.769268701363833074, 3.567999999999999616, -0.3249191361593797289 ) ) ;
#11148 = FACE_OUTER_BOUND ( 'NONE', #13356, .T. ) ;
#11149 = CARTESIAN_POINT ( 'NONE',  ( 4.572644766289085005, 1.800139870985668411, 0.2814996426995059475 ) ) ;
#11151 = VERTEX_POINT ( 'NONE', #5586 ) ;
#11150 = CARTESIAN_POINT ( 'NONE',  ( -5.764454660286586870E-18, 0.000000000000000000, 0.000000000000000000 ) ) ;
#11152 = CONICAL_SURFACE ( 'NONE', #13585, 0.2625000000000000111, 0.7853981633974621568 ) ;
#11153 = ORIENTED_EDGE ( 'NONE', *, *, #1358, .F. ) ;
#11155 = VERTEX_POINT ( 'NONE', #4511 ) ;
#11154 = DIRECTION ( 'NONE',  ( 0.000000000000000000, 0.000000000000000000, -1.000000000000000000 ) ) ;
#11156 = ORIENTED_EDGE ( 'NONE', *, *, #2141, .F. ) ;
#11157 = CARTESIAN_POINT ( 'NONE',  ( 0.4108223460329304411, 4.529999999999999361, -0.2849999999999985323 ) ) ;
#11158 =( CONVERSION_BASED_UNIT ( 'INCH', #6653 ) LENGTH_UNIT ( ) NAMED_UNIT ( #13197 ) );
#11159 = CARTESIAN_POINT ( 'NONE',  ( 3.394491571325183088, -1.679378605318041950, 1.941878605318059003 ) ) ;
#11160 = EDGE_LOOP ( 'NONE', ( #12974, #13416, #7262, #3652 ) ) ;
#11161 = AXIS2_PLACEMENT_3D ( 'NONE', #13722, #865, #2185 ) ;
#11162 = DIRECTION ( 'NONE',  ( 0.000000000000000000, 0.000000000000000000, 1.000000000000000000 ) ) ;
#11163 = CARTESIAN_POINT ( 'NONE',  ( 3.875000000000000000, 3.535499999999999865, 0.4849999999999995981 ) ) ;
#11164 = CARTESIAN_POINT ( 'NONE',  ( 2.001999999999999780, 0.000000000000000000, 0.000000000000000000 ) ) ;
#11165 = PLANE ( 'NONE',  #11612 ) ;
#11166 = DIRECTION ( 'NONE',  ( 0.000000000000000000, 0.000000000000000000, 1.000000000000000000 ) ) ;
#11167 = VERTEX_POINT ( 'NONE', #11471 ) ;
#11168 = LINE ( 'NONE', #7811, #10953 ) ;
#11169 = CARTESIAN_POINT ( 'NONE',  ( 3.759899079166374669, 0.8734932728588881146, -0.4868506001230482050 ) ) ;
#11170 = CARTESIAN_POINT ( 'NONE',  ( 3.394491571325183088, -1.679378605318041950, 1.679378605318059048 ) ) ;
#11171 = ORIENTED_EDGE ( 'NONE', *, *, #4370, .F. ) ;
#11172 = CARTESIAN_POINT ( 'NONE',  ( 0.7006931131589942963, -0.4056294202290754991, 0.4858697363291138438 ) ) ;
#11173 = CARTESIAN_POINT ( 'NONE',  ( 6.794491571325179891, -1.679378605318048390, 2.054378605318054607 ) ) ;
#11174 = ORIENTED_EDGE ( 'NONE', *, *, #9302, .F. ) ;
#11175 = FACE_OUTER_BOUND ( 'NONE', #1480, .T. ) ;
#11176 = ORIENTED_EDGE ( 'NONE', *, *, #1206, .F. ) ;
#11177 = ADVANCED_FACE ( 'NONE', ( #9178 ), #13900, .T. ) ;
#11178 = CYLINDRICAL_SURFACE ( 'NONE', #445, 0.1899999999999996136 ) ;
#11179 = AXIS2_PLACEMENT_3D ( 'NONE', #3084, #1923, #4308 ) ;
#11180 = EDGE_CURVE ( 'NONE', #2919, #3470, #15100, .T. ) ;
#11181 = LINE ( 'NONE', #4668, #7099 ) ;
#11182 = VECTOR ( 'NONE', #4265, 39.37007874015748143 ) ;
#11183 = DIRECTION ( 'NONE',  ( -1.000000000000000000, -0.000000000000000000, -0.000000000000000000 ) ) ;
#11184 = CYLINDRICAL_SURFACE ( 'NONE', #650, 0.2625000000000000111 ) ;
#11185 = CARTESIAN_POINT ( 'NONE',  ( 1.001118301508059583, -0.4429655524010116530, -0.4281838130439684642 ) ) ;
#11186 = EDGE_LOOP ( 'NONE', ( #8308, #14692, #6202, #1290, #1933, #13993 ) ) ;
#11187 = EDGE_CURVE ( 'NONE', #11754, #259, #5838, .T. ) ;
#11188 = AXIS2_PLACEMENT_3D ( 'NONE', #5168, #9616, #3945 ) ;
#11189 = DIRECTION ( 'NONE',  ( -1.000000000000000000, -0.000000000000000000, -0.000000000000000000 ) ) ;
#11190 = DIRECTION ( 'NONE',  ( -1.000000000000000000, -0.000000000000000000, -0.000000000000000000 ) ) ;
#11191 = AXIS2_PLACEMENT_3D ( 'NONE', #7724, #13445, #12382 ) ;
#11192 = DIRECTION ( 'NONE',  ( 0.000000000000000000, 0.000000000000000000, -1.000000000000000000 ) ) ;
#11193 = ORIENTED_EDGE ( 'NONE', *, *, #383, .T. ) ;
#11194 = ORIENTED_EDGE ( 'NONE', *, *, #6907, .T. ) ;
#11195 = CARTESIAN_POINT ( 'NONE',  ( 2.088768908813758873, 0.2870784642939425146, 0.4704976142822915319 ) ) ;
#11196 = VERTEX_POINT ( 'NONE', #6733 ) ;
#11197 = FACE_OUTER_BOUND ( 'NONE', #3787, .T. ) ;
#11198 = VECTOR ( 'NONE', #7446, 39.37007874015748143 ) ;
#11199 = EDGE_CURVE ( 'NONE', #7267, #8189, #9102, .T. ) ;
#11200 = AXIS2_PLACEMENT_3D ( 'NONE', #13240, #6227, #13393 ) ;
#11201 = CARTESIAN_POINT ( 'NONE',  ( 0.7040121242107760802, -0.3870851776472034600, -0.4900563259292263218 ) ) ;
#11202 = CONICAL_SURFACE ( 'NONE', #8040, 3.000000000000000444, 0.7853981633974568277 ) ;
#11203 = EDGE_CURVE ( 'NONE', #13460, #10938, #4821, .T. ) ;
#11204 = VECTOR ( 'NONE', #76, 39.37007874015748143 ) ;
#11205 = DIRECTION ( 'NONE',  ( 0.000000000000000000, 0.000000000000000000, 1.000000000000000000 ) ) ;
#11206 = CARTESIAN_POINT ( 'NONE',  ( 4.203741336932380612, 1.785315657883247864, 0.6766739387161787578 ) ) ;
#11207 = ORIENTED_EDGE ( 'NONE', *, *, #13190, .F. ) ;
#11208 = CIRCLE ( 'NONE', #6579, 0.2944999999999987073 ) ;
#11209 = ADVANCED_FACE ( 'NONE', ( #12832 ), #5508, .T. ) ;
#11210 = B_SPLINE_CURVE_WITH_KNOTS ( 'NONE', 3,
 ( #2629, #4069, #525, #14319, #7439, #11028, #3992, #231, #6151, #7306, #8737, #4933, #3777, #5006, #5152, #9810, #9740, #12027, #8527, #3857, #7588, #11961 ),
 .UNSPECIFIED., .F., .F.,
 ( 4, 2, 2, 2, 2, 2, 2, 2, 2, 2, 4 ),
 ( 2.884201070676985282E-07, 0.0006930185370350131369, 0.001385748653962958453, 0.002771208887818838677, 0.004156669121674718900, 0.005542129355530598690, 0.006927589589386478480, 0.008313049823242359138, 0.009698510057098238060, 0.01039124017402617665, 0.01108397029095411178 ),
 .UNSPECIFIED. ) ;
#11211 = EDGE_LOOP ( 'NONE', ( #11383, #2092, #11695, #2353 ) ) ;
#11212 = ORIENTED_EDGE ( 'NONE', *, *, #6641, .T. ) ;
#11213 = VECTOR ( 'NONE', #12889, 39.37007874015748143 ) ;
#11214 = ADVANCED_FACE ( 'NONE', ( #10177 ), #8191, .F. ) ;
#11215 = ORIENTED_EDGE ( 'NONE', *, *, #12563, .T. ) ;
#11216 = CARTESIAN_POINT ( 'NONE',  ( 0.2448097035962774060, 1.581125151349147107, -0.3378826611373836886 ) ) ;
#11217 = CARTESIAN_POINT ( 'NONE',  ( 3.388087119187628282, 0.7512727810421430119, -0.4521456621583668234 ) ) ;
#11218 = CARTESIAN_POINT ( 'NONE',  ( 3.908162907339028269, 0.8665001417438028541, 0.4991805435374154776 ) ) ;
#11219 = DIRECTION ( 'NONE',  ( -1.000000000000000000, -0.000000000000000000, -0.000000000000000000 ) ) ;
#11220 = EDGE_LOOP ( 'NONE', ( #7922, #8343, #14878, #2412, #7454, #6164 ) ) ;
#11221 = DIRECTION ( 'NONE',  ( 0.2251194151855830106, -0.9743259920144011765, -0.003179652756858232596 ) ) ;
#11222 = CARTESIAN_POINT ( 'NONE',  ( 3.388085670168073715, 0.7513023213622326280, -0.3921396980529558429 ) ) ;
#11223 = DIRECTION ( 'NONE',  ( -0.000000000000000000, -1.000000000000000000, -0.000000000000000000 ) ) ;
#11224 = CONICAL_SURFACE ( 'NONE', #5863, 0.3750000000000007772, 0.7853981633974536081 ) ;
#11225 = DIRECTION ( 'NONE',  ( 0.000000000000000000, 0.000000000000000000, -1.000000000000000000 ) ) ;
#11226 = EDGE_CURVE ( 'NONE', #9279, #14642, #14910, .T. ) ;
#11227 = CONICAL_SURFACE ( 'NONE', #12202, 1.875500000000000167, 0.7853981633974492782 ) ;
#11228 = CARTESIAN_POINT ( 'NONE',  ( 0.9644366315231677200, -0.4455811681533944912, -0.4137692285681027760 ) ) ;
#11229 = DIRECTION ( 'NONE',  ( 0.000000000000000000, 0.000000000000000000, 1.000000000000000000 ) ) ;
#11230 = CARTESIAN_POINT ( 'NONE',  ( 4.121281386195119190, 1.726130368164997320, 0.7563743875758589530 ) ) ;
#11232 = ORIENTED_EDGE ( 'NONE', *, *, #7763, .T. ) ;
#11231 = CARTESIAN_POINT ( 'NONE',  ( 3.715374161931121133, 1.936069962591262517, -0.4743889576438739542 ) ) ;
#11233 = EDGE_CURVE ( 'NONE', #843, #355, #8057, .T. ) ;
#11234 = ADVANCED_FACE ( 'NONE', ( #9033, #14053 ), #196, .F. ) ;
#11235 = EDGE_LOOP ( 'NONE', ( #13794, #764, #1710, #13401 ) ) ;
#11237 = ORIENTED_EDGE ( 'NONE', *, *, #14195, .T. ) ;
#11236 = CARTESIAN_POINT ( 'NONE',  ( 2.156999999999998696, -1.679378605318059048, -1.679378605318041950 ) ) ;
#11238 = ORIENTED_EDGE ( 'NONE', *, *, #3057, .F. ) ;
#11239 = CIRCLE ( 'NONE', #7821, 0.2219999999999999751 ) ;
#11240 = PLANE ( 'NONE',  #10680 ) ;
#11241 = SHAPE_REPRESENTATION_RELATIONSHIP ( 'NONE' , 'NONE' ,  #1600, #5839 ) ;
#11242 = DIRECTION ( 'NONE',  ( 0.000000000000000000, 0.000000000000000000, 1.000000000000000000 ) ) ;
#11243 = VERTEX_POINT ( 'NONE', #10780 ) ;
#11244 = DIRECTION ( 'NONE',  ( 0.000000000000000000, 0.000000000000000000, -1.000000000000000000 ) ) ;
#11245 = DIRECTION ( 'NONE',  ( -1.000000000000000000, 0.000000000000000000, 0.000000000000000000 ) ) ;
#11246 = CARTESIAN_POINT ( 'NONE',  ( 3.471303878679115051, 1.057055486693973645, -0.4509702841989021715 ) ) ;
#11247 = DIRECTION ( 'NONE',  ( -0.000000000000000000, -1.000000000000000000, -0.000000000000000000 ) ) ;
#11248 = EDGE_LOOP ( 'NONE', ( #5292, #14270, #9802, #13075 ) ) ;
#11249 = CARTESIAN_POINT ( 'NONE',  ( 8.066592045432399679E-17, 0.1759999999999999065, 0.7057575716915831521 ) ) ;
#11250 = LINE ( 'NONE', #11321, #289 ) ;
#11251 = CARTESIAN_POINT ( 'NONE',  ( 3.897779889561915567, 1.772923893090484926, -0.7985164159195319300 ) ) ;
#11252 = ORIENTED_EDGE ( 'NONE', *, *, #1553, .F. ) ;
#11253 = EDGE_CURVE ( 'NONE', #7544, #2357, #1431, .T. ) ;
#11254 = CARTESIAN_POINT ( 'NONE',  ( 0.000000000000000000, 0.1749999999999999889, 0.000000000000000000 ) ) ;
#11255 = LINE ( 'NONE', #13834, #15046 ) ;
#11256 = ORIENTED_EDGE ( 'NONE', *, *, #7129, .F. ) ;
#11257 = CARTESIAN_POINT ( 'NONE',  ( 2.124999999999999556, 1.679378605318059048, 1.679378605318041506 ) ) ;
#11258 = AXIS2_PLACEMENT_3D ( 'NONE', #13620, #6172, #11906 ) ;
#11259 = SURFACE_STYLE_USAGE ( .BOTH. , #4304 ) ;
#11260 = DIRECTION ( 'NONE',  ( 0.000000000000000000, 0.000000000000000000, 1.000000000000000000 ) ) ;
#11261 = PRESENTATION_STYLE_ASSIGNMENT (( #4957 ) ) ;
#11262 = CARTESIAN_POINT ( 'NONE',  ( 0.000000000000000000, 1.239999999999999991, 0.000000000000000000 ) ) ;
#11263 = DIRECTION ( 'NONE',  ( 1.000000000000000000, 0.000000000000000000, 0.000000000000000000 ) ) ;
#11264 = VERTEX_POINT ( 'NONE', #1504 ) ;
#11265 = FACE_OUTER_BOUND ( 'NONE', #15079, .T. ) ;
#11266 = CIRCLE ( 'NONE', #10783, 0.5000000000000002220 ) ;
#11267 = CARTESIAN_POINT ( 'NONE',  ( 6.096491571325181269, 0.000000000000000000, 0.000000000000000000 ) ) ;
#11268 = DIRECTION ( 'NONE',  ( 0.4999999999999918954, 0.000000000000000000, -0.8660254037844431485 ) ) ;
#11269 = PRODUCT_RELATED_PRODUCT_CATEGORY ( 'part', '', ( #12024 ) ) ;
#11270 = FACE_OUTER_BOUND ( 'NONE', #6218, .T. ) ;
#11271 = EDGE_LOOP ( 'NONE', ( #14159, #10070, #1264, #14042 ) ) ;
#11272 = EDGE_LOOP ( 'NONE', ( #1517, #7318, #7543, #5404, #12005 ) ) ;
#11273 = CARTESIAN_POINT ( 'NONE',  ( 3.405153689607044232, 3.137999999999999901, -1.491010071662831171 ) ) ;
#11274 = EDGE_LOOP ( 'NONE', ( #6066, #5604, #5941, #6298 ) ) ;
#11275 = CARTESIAN_POINT ( 'NONE',  ( 2.774999999999999911, 1.679378605318059048, 1.679378605318041506 ) ) ;
#11276 = CARTESIAN_POINT ( 'NONE',  ( 0.7070095302585194252, -0.4241756164644422400, -0.4738366780029937275 ) ) ;
#11277 = AXIS2_PLACEMENT_3D ( 'NONE', #14257, #6168, #12120 ) ;
#11278 = DIRECTION ( 'NONE',  ( -0.000000000000000000, 1.000000000000000000, -0.000000000000000000 ) ) ;
#11279 = CARTESIAN_POINT ( 'NONE',  ( 3.851708199487537954, 1.891837914331504944, 0.5000000000000002220 ) ) ;
#11280 = ORIENTED_EDGE ( 'NONE', *, *, #7055, .F. ) ;
#11281 = EDGE_CURVE ( 'NONE', #10474, #9631, #6122, .T. ) ;
#11282 = EDGE_CURVE ( 'NONE', #2531, #4331, #4971, .T. ) ;
#11283 = EDGE_CURVE ( 'NONE', #6554, #4834, #14208, .T. ) ;
#11284 = EDGE_LOOP ( 'NONE', ( #2570, #689, #14950, #9787 ) ) ;
#11285 = ORIENTED_EDGE ( 'NONE', *, *, #14788, .T. ) ;
#11286 = ORIENTED_EDGE ( 'NONE', *, *, #10749, .T. ) ;
#11287 = CARTESIAN_POINT ( 'NONE',  ( 0.1250000000000009992, 0.000000000000000000, 0.000000000000000000 ) ) ;
#11288 = EDGE_CURVE ( 'NONE', #261, #2297, #1276, .T. ) ;
#11289 = CARTESIAN_POINT ( 'NONE',  ( -0.2849999999999999756, 5.750000000000000000, 0.4108223460329293864 ) ) ;
#11290 = DIRECTION ( 'NONE',  ( 0.000000000000000000, 0.000000000000000000, 1.000000000000000000 ) ) ;
#11291 = EDGE_CURVE ( 'NONE', #6251, #3716, #8309, .T. ) ;
#11292 = CONTEXT_DEPENDENT_SHAPE_REPRESENTATION ( #10182, #4952 ) ;
#11293 = CARTESIAN_POINT ( 'NONE',  ( 2.320261876819214919, 0.5185714323020406136, 0.4672279395929489487 ) ) ;
#11294 = EDGE_LOOP ( 'NONE', ( #3300, #3858, #924, #2948 ) ) ;
#11295 = CARTESIAN_POINT ( 'NONE',  ( 3.874999999999999556, 3.137999999999999901, 1.542000000000000037 ) ) ;
#11296 = DIRECTION ( 'NONE',  ( -0.000000000000000000, 1.000000000000000000, -0.000000000000000000 ) ) ;
#11297 = CARTESIAN_POINT ( 'NONE',  ( 0.9884490062245532283, -0.4415602900406226383, -0.4398366647702034449 ) ) ;
#11298 = CARTESIAN_POINT ( 'NONE',  ( 4.527399619855013491, 1.736316896047668701, 0.3745023640388373543 ) ) ;
#11300 = ORIENTED_EDGE ( 'NONE', *, *, #8195, .F. ) ;
#11299 = CARTESIAN_POINT ( 'NONE',  ( 3.474165694507085345, 2.035929352673752302, -0.3024794417911187416 ) ) ;
#11301 = CIRCLE ( 'NONE', #9839, 0.8000000000000000444 ) ;
#11302 = ORIENTED_EDGE ( 'NONE', *, *, #4004, .F. ) ;
#11304 = EDGE_LOOP ( 'NONE', ( #6502, #8273, #8845, #12009 ) ) ;
#11303 = CARTESIAN_POINT ( 'NONE',  ( 0.6784300926939517140, -1.122412978718160259, -0.4304116694862061832 ) ) ;
#11305 = ORIENTED_EDGE ( 'NONE', *, *, #13053, .T. ) ;
#11306 = DIRECTION ( 'NONE',  ( -0.000000000000000000, -1.000000000000000000, -0.000000000000000000 ) ) ;
#11307 = CARTESIAN_POINT ( 'NONE',  ( 3.394491571325182644, 1.679378605318042395, -1.679378605318058604 ) ) ;
#11308 = VERTEX_POINT ( 'NONE', #3676 ) ;
#11309 = AXIS2_PLACEMENT_3D ( 'NONE', #2112, #13502, #877 ) ;
#11310 = DIRECTION ( 'NONE',  ( 0.000000000000000000, 1.000000000000000000, 0.000000000000000000 ) ) ;
#11311 = DIRECTION ( 'NONE',  ( 0.000000000000000000, 0.000000000000000000, 1.000000000000000000 ) ) ;
#11312 = ADVANCED_FACE ( 'NONE', ( #4739 ), #10703, .T. ) ;
#11313 = DIRECTION ( 'NONE',  ( 0.000000000000000000, 0.000000000000000000, -1.000000000000000000 ) ) ;
#11314 = ADVANCED_FACE ( 'NONE', ( #7269 ), #9488, .F. ) ;
#11315 = DIRECTION ( 'NONE',  ( 0.000000000000000000, 0.7071067811865600072, 0.7071067811865350272 ) ) ;
#11316 = B_SPLINE_CURVE_WITH_KNOTS ( 'NONE', 3,
 ( #12439, #2100, #5483, #11448, #4188, #14811, #867, #3193, #4262, #5715, #9156, #2022 ),
 .UNSPECIFIED., .F., .F.,
 ( 4, 2, 2, 2, 2, 4 ),
 ( 3.848605514871169070E-18, 0.001383149773560821052, 0.002766299547121638201, 0.004149449320682454048, 0.004841024207462863924, 0.005532599094243272932 ),
 .UNSPECIFIED. ) ;
#11317 = CARTESIAN_POINT ( 'NONE',  ( 1.007158160401918190, -0.4429913151844830921, -0.4174182184235564197 ) ) ;
#11318 = VERTEX_POINT ( 'NONE', #12913 ) ;
#11319 = LINE ( 'NONE', #588, #13635 ) ;
#11320 = CIRCLE ( 'NONE', #10844, 0.3750000000000007772 ) ;
#11321 = CARTESIAN_POINT ( 'NONE',  ( 2.742999999999999883, -1.679378605318041950, 1.416878605318058870 ) ) ;
#11322 = CARTESIAN_POINT ( 'NONE',  ( 3.426491571325181340, 1.954234464180151676, -0.6847610993685215863 ) ) ;
#11323 = AXIS2_PLACEMENT_3D ( 'NONE', #8817, #11408, #13759 ) ;
#11324 = CLOSED_SHELL ( 'NONE', ( #5543, #7732, #13081, #11813, #6265, #14347, #9143, #7521, #5631, #2916, #12137, #13984, #11484, #13715, #9788, #3732, #5966, #5542, #8492, #4542, #316, #5928, #3067, #11369, #9674, #8662, #11760, #12157, #457, #496, #2798, #7917, #11844, #11314, #6811, #1859, #12365, #6663, #13735, #7577, #13189, #5571, #7126, #14192, #14484, #10940, #7950, #7975, #10687, #3431, #449, #10913, #9615, #6935, #4230, #13289, #9709, #1617, #7279, #9623, #11797, #10584, #13446, #341, #8175, #6582, #13692, #7094, #745, #13925, #12584, #2696, #4915, #9656, #8973, #13330, #4554, #7007, #13904, #5770, #14736, #15015, #13998, #2557, #6602, #4470, #7783, #9819, #14896, #12438, #4958, #1490, #11508, #11925, #4945, #10762, #11209, #2589, #4499, #10650, #9598, #8124, #10740, #12400, #11119, #6341, #10018, #418, #4802, #5597, #5217, #5845, #6350, #630, #5296, #3827, #2229, #7243, #11548, #3554, #7845, #3187, #7616, #13142, #11864, #12957, #6945, #1169, #7976, #12121 ) ) ;
#11325 = CARTESIAN_POINT ( 'NONE',  ( 0.7072875780376983723, -0.4246213910874223063, 0.4734421766419261157 ) ) ;
#11326 = CARTESIAN_POINT ( 'NONE',  ( 1.250000000000000000, 0.000000000000000000, -0.4223386481965726302 ) ) ;
#11327 = EDGE_LOOP ( 'NONE', ( #2336, #13972, #13417, #7589 ) ) ;
#11328 = LINE ( 'NONE', #10194, #9385 ) ;
#11329 = ORIENTED_EDGE ( 'NONE', *, *, #895, .T. ) ;
#11330 = VECTOR ( 'NONE', #7813, 39.37007874015748143 ) ;
#11331 = AXIS2_PLACEMENT_3D ( 'NONE', #1200, #5893, #43 ) ;
#11332 = ADVANCED_FACE ( 'NONE', ( #3895 ), #14356, .T. ) ;
#11333 = CARTESIAN_POINT ( 'NONE',  ( 0.7017867892446607581, -0.4844395604395603239, -0.4010711782184314678 ) ) ;
#11334 = DIRECTION ( 'NONE',  ( 0.000000000000000000, -8.723548215061523903E-15, -1.000000000000000000 ) ) ;
#11335 = DIRECTION ( 'NONE',  ( 0.7071067811865516806, 0.000000000000000000, -0.7071067811865433539 ) ) ;
#11336 = ORIENTED_EDGE ( 'NONE', *, *, #12794, .T. ) ;
#11337 = DIRECTION ( 'NONE',  ( -0.000000000000000000, 1.000000000000000000, -0.000000000000000000 ) ) ;
#11338 = CARTESIAN_POINT ( 'NONE',  ( 2.774999999999999911, -1.679378605318059048, -1.679378605318041950 ) ) ;
#11339 = VECTOR ( 'NONE', #5517, 39.37007874015748143 ) ;
#11340 = CARTESIAN_POINT ( 'NONE',  ( 0.7072031222531457439, -0.4244982521704789291, -0.4735570389444669348 ) ) ;
#11341 = ORIENTED_EDGE ( 'NONE', *, *, #7927, .F. ) ;
#11342 = EDGE_LOOP ( 'NONE', ( #338, #1964, #12727, #8326 ) ) ;
#11343 = DIRECTION ( 'NONE',  ( 0.000000000000000000, 1.000000000000000000, 0.000000000000000000 ) ) ;
#11344 = ORIENTED_EDGE ( 'NONE', *, *, #10917, .F. ) ;
#11345 = CARTESIAN_POINT ( 'NONE',  ( 0.6179999999999965521, 1.679378605318035733, -2.054378605318066153 ) ) ;
#11346 = LINE ( 'NONE', #703, #4196 ) ;
#11347 = DIRECTION ( 'NONE',  ( 0.000000000000000000, 0.000000000000000000, -1.000000000000000000 ) ) ;
#11348 = AXIS2_PLACEMENT_3D ( 'NONE', #2862, #8393, #10901 ) ;
#11349 = FACE_OUTER_BOUND ( 'NONE', #11304, .T. ) ;
#11350 = EDGE_CURVE ( 'NONE', #8027, #13304, #9019, .T. ) ;
#11351 = AXIS2_PLACEMENT_3D ( 'NONE', #14779, #4314, #12792 ) ;
#11352 = CIRCLE ( 'NONE', #14524, 2.499999999999999556 ) ;
#11353 = EDGE_LOOP ( 'NONE', ( #14182, #10446, #5865, #8023 ) ) ;
#11354 = ORIENTED_EDGE ( 'NONE', *, *, #307, .T. ) ;
#11355 = VERTEX_POINT ( 'NONE', #2595 ) ;
#11356 = UNCERTAINTY_MEASURE_WITH_UNIT (LENGTH_MEASURE( 1.000000000000000082E-05 ), #10776, 'distance_accuracy_value', 'NONE');
#11357 = CIRCLE ( 'NONE', #14040, 0.2944999999999987073 ) ;
#11358 = CARTESIAN_POINT ( 'NONE',  ( -0.4273790000699995706, 1.569549437900772393, -0.02166336374279465016 ) ) ;
#11359 = ORIENTED_EDGE ( 'NONE', *, *, #13826, .T. ) ;
#11360 = LINE ( 'NONE', #10148, #8724 ) ;
#11361 = AXIS2_PLACEMENT_3D ( 'NONE', #9949, #738, #13444 ) ;
#11362 = AXIS2_PLACEMENT_3D ( 'NONE', #981, #14276, #4679 ) ;
#11363 = DIRECTION ( 'NONE',  ( -0.7755991921403738720, 0.000000000000000000, 0.6312257069790484509 ) ) ;
#11364 = FACE_OUTER_BOUND ( 'NONE', #12514, .T. ) ;
#11365 = CARTESIAN_POINT ( 'NONE',  ( 3.394491571325182644, 1.679378605318042395, -1.679378605318058604 ) ) ;
#11366 = ORIENTED_EDGE ( 'NONE', *, *, #6713, .T. ) ;
#11367 = CARTESIAN_POINT ( 'NONE',  ( 3.167133238847447352, 2.488124734743586863, 0.2437657924683038213 ) ) ;
#11368 = EDGE_CURVE ( 'NONE', #1017, #2536, #8352, .T. ) ;
#11369 = ADVANCED_FACE ( 'NONE', ( #7194 ), #13872, .F. ) ;
#11370 = FACE_OUTER_BOUND ( 'NONE', #22, .T. ) ;
#11371 = ADVANCED_FACE ( 'NONE', ( #2672 ), #3404, .T. ) ;
#11372 = CARTESIAN_POINT ( 'NONE',  ( 8.792093969802149189, 0.8799778768672790186, 6.829619984160658046E-17 ) ) ;
#11373 = AXIS2_PLACEMENT_3D ( 'NONE', #14533, #13529, #7659 ) ;
#11374 = CONICAL_SURFACE ( 'NONE', #4793, 0.1050000000000001071, 0.7853981633974560506 ) ;
#11375 = CIRCLE ( 'NONE', #609, 1.812000000000000277 ) ;
#11376 = CARTESIAN_POINT ( 'NONE',  ( 4.315797241329101475, 3.137999999999999901, 1.570821732971949825 ) ) ;
#11377 = EDGE_CURVE ( 'NONE', #11969, #6443, #15112, .T. ) ;
#11378 = CARTESIAN_POINT ( 'NONE',  ( 4.392975333536766946, 1.728401786935677142, 0.5451410124394034939 ) ) ;
#11380 = VERTEX_POINT ( 'NONE', #5897 ) ;
#11379 = CARTESIAN_POINT ( 'NONE',  ( 3.521151862607384775, 2.014578117734890927, -0.3540225754882596609 ) ) ;
#11381 = VERTEX_POINT ( 'NONE', #10551 ) ;
#11383 = ORIENTED_EDGE ( 'NONE', *, *, #12184, .F. ) ;
#11382 = DIRECTION ( 'NONE',  ( -0.000000000000000000, -1.000000000000000000, -0.000000000000000000 ) ) ;
#11384 = VERTEX_POINT ( 'NONE', #48 ) ;
#11385 = CARTESIAN_POINT ( 'NONE',  ( 0.3725000000000000533, 0.1749999999999999889, -0.4124999999999999778 ) ) ;
#11386 = CIRCLE ( 'NONE', #4804, 0.5175000000000000711 ) ;
#11387 = CARTESIAN_POINT ( 'NONE',  ( 3.388933043275772494, 0.7513023213622327390, -0.4521337140780258279 ) ) ;
#11388 = ORIENTED_EDGE ( 'NONE', *, *, #3237, .F. ) ;
#11389 = CARTESIAN_POINT ( 'NONE',  ( 2.775039370078740131, 1.679378605318059492, 1.304378605318041062 ) ) ;
#11390 = DIRECTION ( 'NONE',  ( -0.3420201433256623846, 0.000000000000000000, -0.9396926207859106484 ) ) ;
#11391 = ADVANCED_FACE ( 'NONE', ( #9413 ), #11141, .T. ) ;
#11392 = AXIS2_PLACEMENT_3D ( 'NONE', #12416, #2321, #8314 ) ;
#11393 = CARTESIAN_POINT ( 'NONE',  ( -0.0008473731076987472792, -0.3830000000000000626, -0.4400059839749300150 ) ) ;
#11394 = CARTESIAN_POINT ( 'NONE',  ( 0.7513246802501661881, 0.05999999999999999778, -0.4293820849162031661 ) ) ;
#11395 = DIRECTION ( 'NONE',  ( 0.000000000000000000, 0.000000000000000000, 1.000000000000000000 ) ) ;
#11396 = ORIENTED_EDGE ( 'NONE', *, *, #4389, .F. ) ;
#11397 = VECTOR ( 'NONE', #14202, 39.37007874015748143 ) ;
#11398 = DIRECTION ( 'NONE',  ( -0.000000000000000000, -1.000000000000000000, -0.000000000000000000 ) ) ;
#11399 = CARTESIAN_POINT ( 'NONE',  ( 3.537273379829105391, 1.962792557789169390, 0.3716385091526580031 ) ) ;
#11400 = CARTESIAN_POINT ( 'NONE',  ( 3.992613899125291521, 1.750100385050365137, -0.7873164154455231101 ) ) ;
#11401 = EDGE_CURVE ( 'NONE', #9366, #9279, #2661, .T. ) ;
#11402 = CARTESIAN_POINT ( 'NONE',  ( 0.7023896125859220296, -0.3918271903216897778, 0.4896155492289064881 ) ) ;
#11403 = CIRCLE ( 'NONE', #8491, 0.1520000000000001905 ) ;
#11405 = EDGE_LOOP ( 'NONE', ( #10164, #4579, #8428, #5687 ) ) ;
#11404 = CARTESIAN_POINT ( 'NONE',  ( 0.8999999999999998002, 0.01999999999999975409, -0.4650000000000000244 ) ) ;
#11406 = VERTEX_POINT ( 'NONE', #13575 ) ;
#11407 = EDGE_CURVE ( 'NONE', #3130, #2748, #13640, .T. ) ;
#11408 = DIRECTION ( 'NONE',  ( -0.000000000000000000, -1.000000000000000000, -0.000000000000000000 ) ) ;
#11409 = ORIENTED_EDGE ( 'NONE', *, *, #6485, .T. ) ;
#11410 = CARTESIAN_POINT ( 'NONE',  ( 0.000000000000000000, 0.000000000000000000, -0.8000000000000000444 ) ) ;
#11411 = CARTESIAN_POINT ( 'NONE',  ( 0.7513246802501664101, -0.4429999999999999494, -0.4293820849162031106 ) ) ;
#11412 = LINE ( 'NONE', #9052, #5248 ) ;
#11413 = CARTESIAN_POINT ( 'NONE',  ( 0.000000000000000000, 1.239999999999999991, 0.000000000000000000 ) ) ;
#11414 = VECTOR ( 'NONE', #6812, 39.37007874015748143 ) ;
#11415 = VERTEX_POINT ( 'NONE', #14433 ) ;
#11416 = CARTESIAN_POINT ( 'NONE',  ( -0.3725000000000000533, 0.1859999999999983611, 0.4124999999999999223 ) ) ;
#11417 = CARTESIAN_POINT ( 'NONE',  ( 2.124999999999999556, 1.575000000000000178, -2.360000000000016751 ) ) ;
#11418 = DIRECTION ( 'NONE',  ( 1.000000000000000000, 0.000000000000000000, 0.000000000000000000 ) ) ;
#11419 = VERTEX_POINT ( 'NONE', #10011 ) ;
#11420 = DIRECTION ( 'NONE',  ( 0.000000000000000000, 1.000000000000000000, -0.000000000000000000 ) ) ;
#11421 = DIRECTION ( 'NONE',  ( -0.000000000000000000, -1.000000000000000000, -0.000000000000000000 ) ) ;
#11422 = EDGE_CURVE ( 'NONE', #167, #9866, #4138, .T. ) ;
#11423 = CIRCLE ( 'NONE', #6836, 0.5000000000000001110 ) ;
#11424 = EDGE_CURVE ( 'NONE', #8576, #6919, #10997, .T. ) ;
#11425 = CARTESIAN_POINT ( 'NONE',  ( 2.806999999999999496, -1.679378605318041950, 1.416878605318058870 ) ) ;
#11426 = ORIENTED_EDGE ( 'NONE', *, *, #1110, .F. ) ;
#11427 = DIRECTION ( 'NONE',  ( -1.000000000000000000, 0.000000000000000000, 0.000000000000000000 ) ) ;
#11428 = CONICAL_SURFACE ( 'NONE', #6311, 0.3750000000000004996, 0.7853981633974589371 ) ;
#11429 = CARTESIAN_POINT ( 'NONE',  ( 0.000000000000000000, 0.1749999999999999889, 0.000000000000000000 ) ) ;
#11430 = CARTESIAN_POINT ( 'NONE',  ( 2.774999999999999911, 1.575000000000016387, 2.359999999999999876 ) ) ;
#11431 = CARTESIAN_POINT ( 'NONE',  ( 3.426491571325181340, 2.058905028113295455, 0.2209981660730358233 ) ) ;
#11432 = AXIS2_PLACEMENT_3D ( 'NONE', #13175, #6304, #2711 ) ;
#11433 = EDGE_LOOP ( 'NONE', ( #14812, #9438, #4710, #2858 ) ) ;
#11434 = AXIS2_PLACEMENT_3D ( 'NONE', #10471, #14048, #11773 ) ;
#11435 = CARTESIAN_POINT ( 'NONE',  ( 3.621938390628993254, 1.891483488391046519, -0.7066767728939699067 ) ) ;
#11436 = VERTEX_POINT ( 'NONE', #8782 ) ;
#11437 = CIRCLE ( 'NONE', #2414, 0.3190000000000000058 ) ;
#11438 = ORIENTED_EDGE ( 'NONE', *, *, #12985, .F. ) ;
#11439 = AXIS2_PLACEMENT_3D ( 'NONE', #5126, #13208, #1509 ) ;
#11440 = ADVANCED_FACE ( 'NONE', ( #5183 ), #12188, .T. ) ;
#11441 = CARTESIAN_POINT ( 'NONE',  ( -0.4019514777495646340, 1.589927591219160830, -0.06570512431237962581 ) ) ;
#11442 = ORIENTED_EDGE ( 'NONE', *, *, #8733, .F. ) ;
#11443 = AXIS2_PLACEMENT_3D ( 'NONE', #13801, #3031, #9011 ) ;
#11444 = CARTESIAN_POINT ( 'NONE',  ( 3.874999999999999556, 2.782000000000002693, 1.320000000000000062 ) ) ;
#11445 = FACE_OUTER_BOUND ( 'NONE', #11580, .T. ) ;
#11447 = CARTESIAN_POINT ( 'NONE',  ( 0.7819547768050734149, -0.4450707063672663111, -0.3325235620832113770 ) ) ;
#11446 = AXIS2_PLACEMENT_3D ( 'NONE', #5609, #5913, #7891 ) ;
#11448 = CARTESIAN_POINT ( 'NONE',  ( -0.07259084472369319030, 1.600827197418697390, 0.3809527529760087794 ) ) ;
#11449 = VERTEX_POINT ( 'NONE', #12143 ) ;
#11450 = DIRECTION ( 'NONE',  ( 0.3420201433256627732, 0.000000000000000000, -0.9396926207859105373 ) ) ;
#11451 = CARTESIAN_POINT ( 'NONE',  ( 0.7022716438625531410, -0.02843846521930830026, -0.4812718407965440592 ) ) ;
#11452 = AXIS2_PLACEMENT_3D ( 'NONE', #9205, #11800, #14083 ) ;
#11453 = AXIS2_PLACEMENT_3D ( 'NONE', #12222, #10709, #6048 ) ;
#11454 = AXIS2_PLACEMENT_3D ( 'NONE', #9959, #14614, #8812 ) ;
#11455 = AXIS2_PLACEMENT_3D ( 'NONE', #5738, #5663, #11390 ) ;
#11456 = CARTESIAN_POINT ( 'NONE',  ( 2.774999999999999911, 1.679378605318059048, 1.679378605318041506 ) ) ;
#11457 = VECTOR ( 'NONE', #1575, 39.37007874015748143 ) ;
#11458 = CARTESIAN_POINT ( 'NONE',  ( 4.641150712690939706, 1.726156072897443661, -0.2600928543580103836 ) ) ;
#11459 = EDGE_CURVE ( 'NONE', #4426, #9791, #3393, .T. ) ;
#11461 = VERTEX_POINT ( 'NONE', #6340 ) ;
#11460 = DIRECTION ( 'NONE',  ( -0.000000000000000000, -1.000000000000000000, -0.000000000000000000 ) ) ;
#11462 = ORIENTED_EDGE ( 'NONE', *, *, #5218, .F. ) ;
#11464 = ORIENTED_EDGE ( 'NONE', *, *, #6288, .T. ) ;
#11463 = CARTESIAN_POINT ( 'NONE',  ( 3.394491571325183088, -1.679378605318041950, 1.416878605318058870 ) ) ;
#11465 = ORIENTED_EDGE ( 'NONE', *, *, #12662, .T. ) ;
#11466 = LINE ( 'NONE', #7800, #11685 ) ;
#11467 = CARTESIAN_POINT ( 'NONE',  ( 2.774999999999999911, -1.679378605318041950, 1.679378605318059048 ) ) ;
#11468 = VERTEX_POINT ( 'NONE', #13495 ) ;
#11469 = COLOUR_RGB ( '',0.7921568627450980005, 0.8196078431372548767, 0.9333333333333333481 ) ;
#11470 = CARTESIAN_POINT ( 'NONE',  ( 2.774999999999999911, 2.360000000000015863, 1.574999999999999956 ) ) ;
#11471 = CARTESIAN_POINT ( 'NONE',  ( 3.875000000000000444, 1.884022191776434152, -0.5000000000000002220 ) ) ;
#11472 = CIRCLE ( 'NONE', #1447, 0.7057575716915831521 ) ;
#11473 = CARTESIAN_POINT ( 'NONE',  ( 0.3725000000000000533, 0.1749999999999999889, -0.3724999999999999978 ) ) ;
#11474 = DIRECTION ( 'NONE',  ( 0.000000000000000000, 0.000000000000000000, -1.000000000000000000 ) ) ;
#11475 = FACE_OUTER_BOUND ( 'NONE', #6781, .T. ) ;
#11476 = FACE_OUTER_BOUND ( 'NONE', #14676, .T. ) ;
#11477 = DIRECTION ( 'NONE',  ( -1.000000000000000000, -0.000000000000000000, -0.000000000000000000 ) ) ;
#11478 = DIRECTION ( 'NONE',  ( -1.000000000000000000, -0.000000000000000000, -0.000000000000000000 ) ) ;
#11479 = CARTESIAN_POINT ( 'NONE',  ( 3.392289215558335957, 0.9914592393105061685, -0.1313972205204200216 ) ) ;
#11480 = EDGE_CURVE ( 'NONE', #1422, #14862, #640, .T. ) ;
#11481 = DIRECTION ( 'NONE',  ( -0.000000000000000000, -1.000000000000000000, -0.000000000000000000 ) ) ;
#11482 = VECTOR ( 'NONE', #9813, 39.37007874015748143 ) ;
#11483 = EDGE_CURVE ( 'NONE', #2425, #1772, #9928, .T. ) ;
#11484 = ADVANCED_FACE ( 'NONE', ( #1721 ), #11943, .F. ) ;
#11485 = DIRECTION ( 'NONE',  ( 0.000000000000000000, 0.000000000000000000, -1.000000000000000000 ) ) ;
#11487 = ORIENTED_EDGE ( 'NONE', *, *, #4113, .F. ) ;
#11486 = DIRECTION ( 'NONE',  ( -1.000000000000000000, 0.000000000000000000, 0.000000000000000000 ) ) ;
#11488 = ORIENTED_EDGE ( 'NONE', *, *, #582, .F. ) ;
#11489 = CARTESIAN_POINT ( 'NONE',  ( -0.4425000000000005596, 0.2159999999999999420, 0.3724999999999999423 ) ) ;
#11490 = ORIENTED_EDGE ( 'NONE', *, *, #10895, .F. ) ;
#11491 = CARTESIAN_POINT ( 'NONE',  ( 3.426491571325181340, 0.000000000000000000, 0.000000000000000000 ) ) ;
#11492 = EDGE_CURVE ( 'NONE', #6091, #11308, #6409, .T. ) ;
#11493 = DIRECTION ( 'NONE',  ( 0.000000000000000000, -0.7071067811865568986, -0.7071067811865381358 ) ) ;
#11494 = EDGE_CURVE ( 'NONE', #9564, #11740, #7703, .T. ) ;
#11495 = CARTESIAN_POINT ( 'NONE',  ( 1.250000000000000000, 0.000000000000000000, 0.4223386481965726857 ) ) ;
#11496 = CARTESIAN_POINT ( 'NONE',  ( 0.000000000000000000, 1.591999999999999638, 0.000000000000000000 ) ) ;
#11497 = CARTESIAN_POINT ( 'NONE',  ( 2.781172880863636303E-17, 0.000000000000000000, -0.2041999999999996596 ) ) ;
#11498 = ORIENTED_EDGE ( 'NONE', *, *, #12903, .F. ) ;
#11499 = DIRECTION ( 'NONE',  ( 0.9943395781194692695, 0.000000000000000000, -0.1062487806292197745 ) ) ;
#11500 = FACE_OUTER_BOUND ( 'NONE', #7716, .T. ) ;
#11501 = ORIENTED_EDGE ( 'NONE', *, *, #1413, .T. ) ;
#11502 = CARTESIAN_POINT ( 'NONE',  ( 0.7441558489118157427, -0.4430000000000000049, -0.4356293359425710832 ) ) ;
#11503 = EDGE_LOOP ( 'NONE', ( #2238, #14901, #1377, #10296 ) ) ;
#11504 = CARTESIAN_POINT ( 'NONE',  ( 3.426491571325181340, 2.360000000000000320, -0.9800000000000009814 ) ) ;
#11505 = CARTESIAN_POINT ( 'NONE',  ( 3.874999999999999556, 3.137999999999999901, -1.320000000000000062 ) ) ;
#11506 = VERTEX_POINT ( 'NONE', #11064 ) ;
#11507 = CARTESIAN_POINT ( 'NONE',  ( 3.314866445692599584, 0.7487158587810271992, 0.4531798524619689017 ) ) ;
#11508 = ADVANCED_FACE ( 'NONE', ( #7553 ), #13427, .T. ) ;
#11509 = CARTESIAN_POINT ( 'NONE',  ( 0.8622576496911000810, -0.4326094837641099589, -0.4616145281884125873 ) ) ;
#11510 = EDGE_CURVE ( 'NONE', #3105, #7097, #677, .T. ) ;
#11511 = LINE ( 'NONE', #5632, #7326 ) ;
#11512 = VECTOR ( 'NONE', #14194, 39.37007874015748143 ) ;
#11513 = EDGE_CURVE ( 'NONE', #14596, #9885, #4266, .T. ) ;
#11514 = FACE_OUTER_BOUND ( 'NONE', #7603, .T. ) ;
#11515 = CARTESIAN_POINT ( 'NONE',  ( 4.049162079869311981, 1.738313153752170992, -0.7765995666616979376 ) ) ;
#11516 = ORIENTED_EDGE ( 'NONE', *, *, #985, .T. ) ;
#11517 = ORIENTED_EDGE ( 'NONE', *, *, #255, .F. ) ;
#11518 = DIRECTION ( 'NONE',  ( 0.000000000000000000, 0.000000000000000000, -1.000000000000000000 ) ) ;
#11519 = EDGE_LOOP ( 'NONE', ( #3789, #9168, #13851, #13270 ) ) ;
#11520 = AXIS2_PLACEMENT_3D ( 'NONE', #13665, #168, #2159 ) ;
#11521 = CARTESIAN_POINT ( 'NONE',  ( 0.5400755080658357077, 0.1749999999999999889, -1.532626322880899838 ) ) ;
#11522 = DIRECTION ( 'NONE',  ( -1.000000000000000000, -0.000000000000000000, -0.000000000000000000 ) ) ;
#11523 = DIRECTION ( 'NONE',  ( -0.000000000000000000, -1.000000000000000000, 0.000000000000000000 ) ) ;
#11524 = FACE_OUTER_BOUND ( 'NONE', #6651, .T. ) ;
#11525 = ORIENTED_EDGE ( 'NONE', *, *, #10181, .F. ) ;
#11526 = LINE ( 'NONE', #1025, #9281 ) ;
#11527 = CARTESIAN_POINT ( 'NONE',  ( 0.6773748815706879256, -0.06659206035557820036, -0.4904325581699052750 ) ) ;
#11528 =( NAMED_UNIT ( * ) PLANE_ANGLE_UNIT ( ) SI_UNIT ( $, .RADIAN. ) );
#11529 = EDGE_CURVE ( 'NONE', #8673, #14941, #13894, .T. ) ;
#11530 = VECTOR ( 'NONE', #5409, 39.37007874015748143 ) ;
#11531 = DIRECTION ( 'NONE',  ( -1.000000000000000000, -0.000000000000000000, -0.000000000000000000 ) ) ;
#11532 = CARTESIAN_POINT ( 'NONE',  ( 4.626491436490355547, 1.749163294474629149, 0.03662930866317349460 ) ) ;
#11533 = ORIENTED_EDGE ( 'NONE', *, *, #6439, .T. ) ;
#11535 = EDGE_LOOP ( 'NONE', ( #3050, #535, #2253, #10025 ) ) ;
#11534 = CARTESIAN_POINT ( 'NONE',  ( 2.774999999999999911, 0.000000000000000000, 0.000000000000000000 ) ) ;
#11536 = APPLICATION_CONTEXT ( 'automotive_design' ) ;
#11537 = VERTEX_POINT ( 'NONE', #11295 ) ;
#11539 = ORIENTED_EDGE ( 'NONE', *, *, #3765, .T. ) ;
#11538 = DIRECTION ( 'NONE',  ( -0.000000000000000000, -1.000000000000000000, -0.000000000000000000 ) ) ;
#11540 = ORIENTED_EDGE ( 'NONE', *, *, #8402, .T. ) ;
#11541 = DIRECTION ( 'NONE',  ( -0.000000000000000000, -0.000000000000000000, -1.000000000000000000 ) ) ;
#11542 = DIRECTION ( 'NONE',  ( 0.000000000000000000, 0.000000000000000000, -1.000000000000000000 ) ) ;
#11543 = ORIENTED_EDGE ( 'NONE', *, *, #11087, .T. ) ;
#11544 = DIRECTION ( 'NONE',  ( 0.000000000000000000, 0.000000000000000000, 1.000000000000000000 ) ) ;
#11545 = DIRECTION ( 'NONE',  ( -1.000000000000000000, -0.000000000000000000, -0.000000000000000000 ) ) ;
#11546 = DIRECTION ( 'NONE',  ( 0.000000000000000000, 0.000000000000000000, 1.000000000000000000 ) ) ;
#11547 = LINE ( 'NONE', #9103, #6688 ) ;
#11548 = ADVANCED_FACE ( 'NONE', ( #9013 ), #1912, .F. ) ;
#11549 = DIRECTION ( 'NONE',  ( 0.000000000000000000, 0.000000000000000000, 1.000000000000000000 ) ) ;
#11550 = VECTOR ( 'NONE', #14312, 39.37007874015748143 ) ;
#11551 = CARTESIAN_POINT ( 'NONE',  ( 3.873439288382781065, 3.137999999999999901, 6.065921084684207584E-32 ) ) ;
#11552 = CARTESIAN_POINT ( 'NONE',  ( -0.2849999999999999756, 5.750000000000000000, -0.4108223460329293864 ) ) ;
#11553 =( BOUNDED_SURFACE ( )  B_SPLINE_SURFACE ( 3, 2, ( 
 ( #5421, #238, #1317 ),
 ( #8456, #14545, #9815 ),
 ( #604, #12104, #4075 ),
 ( #8742, #7666, #13390 ),
 ( #14706, #5756, #12543 ),
 ( #2066, #9121, #1921 ),
 ( #11566, #3305, #7978 ),
 ( #6606, #4531, #9203 ),
 ( #13843, #3383, #1069 ),
 ( #6987, #11049, #13481 ) ),
 .UNSPECIFIED., .F., .F., .F. ) 
 B_SPLINE_SURFACE_WITH_KNOTS ( ( 4, 2, 2, 2, 4 ),
 ( 3, 3 ),
 ( 4.712388980384689674, 4.908738521234050189, 5.105088062083410705, 5.301437602932772108, 5.497787143782132624 ),
 ( 0.000000000000000000, 1.000000000000000000 ),
 .UNSPECIFIED. ) 
 GEOMETRIC_REPRESENTATION_ITEM ( )  RATIONAL_B_SPLINE_SURFACE ( (
 ( 1.000000000000000000, 0.7071067811865475727, 1.000000000000000000),
 ( 1.000000000000000000, 0.7074335897363954739, 1.000000000000000000),
 ( 1.000000000000000000, 0.7077601512488349567, 1.000000000000000000),
 ( 1.000000000000000000, 0.7084003186185308110, 1.000000000000000000),
 ( 1.000000000000000000, 0.7087139042191036298, 1.000000000000000000),
 ( 1.000000000000000000, 0.7093161336544245854, 1.000000000000000000),
 ( 1.000000000000000000, 0.7096047632059221399, 1.000000000000000000),
 ( 1.000000000000000000, 0.7101460984466749782, 1.000000000000000000),
 ( 1.000000000000000000, 0.7103988163344383544, 1.000000000000000000),
 ( 1.000000000000000000, 0.7106287314217416551, 1.000000000000000000) ) ) 
 REPRESENTATION_ITEM ( '' )  SURFACE ( )  );
#11554 = CARTESIAN_POINT ( 'NONE',  ( 3.401947036691211679, 0.9867933195744326147, 0.1627677899319876775 ) ) ;
#11555 = CARTESIAN_POINT ( 'NONE',  ( 4.313863554662043853, 1.707918880701486009, 0.6659606377349818196 ) ) ;
#11556 = DIRECTION ( 'NONE',  ( 0.000000000000000000, 0.000000000000000000, -1.000000000000000000 ) ) ;
#11558 = EDGE_LOOP ( 'NONE', ( #2752, #14678, #14883, #7018 ) ) ;
#11557 = DIRECTION ( 'NONE',  ( 1.000000000000000000, 0.000000000000000000, 0.000000000000000000 ) ) ;
#11559 = ORIENTED_EDGE ( 'NONE', *, *, #11674, .F. ) ;
#11560 = CARTESIAN_POINT ( 'NONE',  ( 0.6733268703976358349, 0.02909690080488760294, -0.4545075337565437912 ) ) ;
#11561 = ORIENTED_EDGE ( 'NONE', *, *, #8516, .T. ) ;
#11562 = DIRECTION ( 'NONE',  ( 0.000000000000000000, 0.000000000000000000, 1.000000000000000000 ) ) ;
#11563 = CARTESIAN_POINT ( 'NONE',  ( 3.320735777595769989, 0.6889667851712865110, -0.4530969522937798311 ) ) ;
#11564 = EDGE_CURVE ( 'NONE', #4411, #3205, #10230, .T. ) ;
#11565 = EDGE_CURVE ( 'NONE', #12994, #13095, #10970, .T. ) ;
#11566 = CARTESIAN_POINT ( 'NONE',  ( 2.002301348309616813, -0.1786631980419839394, 0.4121376268991519543 ) ) ;
#11567 = CARTESIAN_POINT ( 'NONE',  ( 3.426491571325181340, 2.360000000000000320, -0.9800000000000009814 ) ) ;
#11568 = EDGE_CURVE ( 'NONE', #13246, #4996, #12919, .T. ) ;
#11569 = AXIS2_PLACEMENT_3D ( 'NONE', #2197, #12975, #11693 ) ;
#11570 = LINE ( 'NONE', #5916, #10475 ) ;
#11571 = ORIENTED_EDGE ( 'NONE', *, *, #7380, .T. ) ;
#11572 = CIRCLE ( 'NONE', #3513, 0.5174999999999995159 ) ;
#11573 = FACE_OUTER_BOUND ( 'NONE', #550, .T. ) ;
#11574 = FACE_OUTER_BOUND ( 'NONE', #1216, .T. ) ;
#11575 = ORIENTED_EDGE ( 'NONE', *, *, #6233, .T. ) ;
#11576 = EDGE_CURVE ( 'NONE', #2690, #13739, #1957, .T. ) ;
#11577 = DIRECTION ( 'NONE',  ( -1.000000000000000000, -0.000000000000000000, -0.000000000000000000 ) ) ;
#11578 = EDGE_LOOP ( 'NONE', ( #14032, #2458, #10193, #9955 ) ) ;
#11579 = FACE_OUTER_BOUND ( 'NONE', #12336, .T. ) ;
#11580 = EDGE_LOOP ( 'NONE', ( #177, #3854, #4927, #10293 ) ) ;
#11581 = VECTOR ( 'NONE', #7128, 39.37007874015748143 ) ;
#11582 = DIRECTION ( 'NONE',  ( -0.000000000000000000, 0.000000000000000000, -1.000000000000000000 ) ) ;
#11583 = CARTESIAN_POINT ( 'NONE',  ( 2.774999999999999911, 2.360000000000000320, -0.9800000000000007594 ) ) ;
#11584 = CARTESIAN_POINT ( 'NONE',  ( 4.215098385813337067, 1.784975328382307769, -0.6693622412112683051 ) ) ;
#11585 = AXIS2_PLACEMENT_3D ( 'NONE', #3213, #894, #4439 ) ;
#11586 = DIRECTION ( 'NONE',  ( 0.000000000000000000, 0.000000000000000000, 1.000000000000000000 ) ) ;
#11587 = PRODUCT_DEFINITION_FORMATION_WITH_SPECIFIED_SOURCE ( 'ANY', '', #9828, .NOT_KNOWN. ) ;
#11588 = CARTESIAN_POINT ( 'NONE',  ( 3.706496129713269916, 1.834319089984349116, -0.7862230264085732223 ) ) ;
#11589 = ORIENTED_EDGE ( 'NONE', *, *, #5525, .T. ) ;
#11590 = ORIENTED_EDGE ( 'NONE', *, *, #4165, .T. ) ;
#11591 = EDGE_CURVE ( 'NONE', #5637, #3175, #12199, .T. ) ;
#11592 = CARTESIAN_POINT ( 'NONE',  ( 3.388085670168073715, 0.7513023213622326280, 0.3921396980529558429 ) ) ;
#11593 = VERTEX_POINT ( 'NONE', #10303 ) ;
#11594 = DIRECTION ( 'NONE',  ( -0.000000000000000000, -1.000000000000000000, -0.000000000000000000 ) ) ;
#11595 = CARTESIAN_POINT ( 'NONE',  ( 0.9482181556124942290, -0.4760276150436455467, -0.4328224131969262700 ) ) ;
#11596 =( NAMED_UNIT ( * ) SI_UNIT ( $, .STERADIAN. ) SOLID_ANGLE_UNIT ( ) );
#11597 = EDGE_CURVE ( 'NONE', #6053, #9069, #11526, .T. ) ;
#11598 = VECTOR ( 'NONE', #5626, 39.37007874015748143 ) ;
#11599 = DIRECTION ( 'NONE',  ( 0.000000000000000000, 0.000000000000000000, 1.000000000000000000 ) ) ;
#11600 = ORIENTED_EDGE ( 'NONE', *, *, #2043, .F. ) ;
#11601 = CARTESIAN_POINT ( 'NONE',  ( 3.161631830458323744, 2.489685336282108086, -0.2285170720271093858 ) ) ;
#11602 = VERTEX_POINT ( 'NONE', #8059 ) ;
#11603 = DIRECTION ( 'NONE',  ( 0.000000000000000000, 0.000000000000000000, 1.000000000000000000 ) ) ;
#11604 = CARTESIAN_POINT ( 'NONE',  ( 3.394491571325180423, -1.679378605318059048, -1.679378605318041950 ) ) ;
#11605 = DIRECTION ( 'NONE',  ( 0.000000000000000000, 1.000000000000000000, 0.000000000000000000 ) ) ;
#11606 = CIRCLE ( 'NONE', #2815, 0.5000000000000001110 ) ;
#11607 = CARTESIAN_POINT ( 'NONE',  ( 4.682886128176067864, 1.732772449459274888, 0.07708318348993609126 ) ) ;
#11608 = EDGE_LOOP ( 'NONE', ( #1367, #7599, #9403, #1094, #246 ) ) ;
#11609 = CIRCLE ( 'NONE', #3797, 1.000000000000000222 ) ;
#11611 = ORIENTED_EDGE ( 'NONE', *, *, #9331, .F. ) ;
#11610 = CARTESIAN_POINT ( 'NONE',  ( 0.4108223460329283871, 4.529999999999999361, 0.2850000000000009748 ) ) ;
#11612 = AXIS2_PLACEMENT_3D ( 'NONE', #665, #5366, #10032 ) ;
#11613 = VERTEX_POINT ( 'NONE', #9158 ) ;
#11615 = VERTEX_POINT ( 'NONE', #12505 ) ;
#11614 = CARTESIAN_POINT ( 'NONE',  ( -0.4125000000000000333, -0.6290000000000005587, 0.4124999999999999223 ) ) ;
#11616 = ORIENTED_EDGE ( 'NONE', *, *, #6620, .F. ) ;
#11617 = EDGE_CURVE ( 'NONE', #9682, #12994, #789, .T. ) ;
#11618 = EDGE_CURVE ( 'NONE', #10168, #1992, #7805, .T. ) ;
#11619 = CARTESIAN_POINT ( 'NONE',  ( 0.4349147617188415249, 0.7512260236060024354, 0.008611041693268213504 ) ) ;
#11620 = ORIENTED_EDGE ( 'NONE', *, *, #14212, .T. ) ;
#11621 = CARTESIAN_POINT ( 'NONE',  ( 4.769268701363833074, 3.137999999999999901, 0.3249191361593796734 ) ) ;
#11622 = CARTESIAN_POINT ( 'NONE',  ( 0.6552635435737790282, -0.4101955659814244814, -0.5075266421723672039 ) ) ;
#11623 = VECTOR ( 'NONE', #1535, 39.37007874015748143 ) ;
#11624 = LINE ( 'NONE', #1208, #15142 ) ;
#11625 = LINE ( 'NONE', #10482, #7906 ) ;
#11626 = AXIS2_PLACEMENT_3D ( 'NONE', #14755, #970, #10400 ) ;
#11627 = DIRECTION ( 'NONE',  ( 0.7071067811865429098, 0.000000000000000000, -0.7071067811865521247 ) ) ;
#11628 = VECTOR ( 'NONE', #10861, 39.37007874015748854 ) ;
#11629 = DIRECTION ( 'NONE',  ( -0.000000000000000000, -1.000000000000000000, -0.000000000000000000 ) ) ;
#11630 = CARTESIAN_POINT ( 'NONE',  ( 3.426491571325181340, -2.399999999999999911, 0.7000000000000007327 ) ) ;
#11631 = LINE ( 'NONE', #4674, #432 ) ;
#11632 = CARTESIAN_POINT ( 'NONE',  ( 3.697049110852476339, 0.8839984663495870088, 0.4675429765723205788 ) ) ;
#11633 = CARTESIAN_POINT ( 'NONE',  ( 0.2249147617188448078, 1.239999999999999991, 0.3723417112827345221 ) ) ;
#11634 = AXIS2_PLACEMENT_3D ( 'NONE', #14222, #210, #11722 ) ;
#11635 = ORIENTED_EDGE ( 'NONE', *, *, #7488, .F. ) ;
#11636 = DIRECTION ( 'NONE',  ( 0.000000000000000000, 0.000000000000000000, 1.000000000000000000 ) ) ;
#11638 = ORIENTED_EDGE ( 'NONE', *, *, #4195, .T. ) ;
#11637 = DIRECTION ( 'NONE',  ( 0.000000000000000000, -0.000000000000000000, -1.000000000000000000 ) ) ;
#11639 = ORIENTED_EDGE ( 'NONE', *, *, #13429, .T. ) ;
#11640 = AXIS2_PLACEMENT_3D ( 'NONE', #6411, #9850, #5259 ) ;
#11641 = AXIS2_PLACEMENT_3D ( 'NONE', #11750, #1249, #5935 ) ;
#11642 = CARTESIAN_POINT ( 'NONE',  ( 0.7017867892446607581, 0.04143956043956044388, -0.4010711782184314678 ) ) ;
#11643 = ORIENTED_EDGE ( 'NONE', *, *, #8215, .T. ) ;
#11644 = DIRECTION ( 'NONE',  ( 0.000000000000000000, 0.000000000000000000, -1.000000000000000000 ) ) ;
#11645 = AXIS2_PLACEMENT_3D ( 'NONE', #2510, #188, #8345 ) ;
#11646 = DIRECTION ( 'NONE',  ( 0.000000000000000000, 0.000000000000000000, -1.000000000000000000 ) ) ;
#11647 = CARTESIAN_POINT ( 'NONE',  ( 0.7500000000000001110, 1.000000000000000000, -1.000000000000000000 ) ) ;
#11648 = ORIENTED_EDGE ( 'NONE', *, *, #1453, .T. ) ;
#11649 = CARTESIAN_POINT ( 'NONE',  ( 0.6592465977460899573, -0.4437463589180128953, 0.4884267951992171675 ) ) ;
#11650 = CARTESIAN_POINT ( 'NONE',  ( 0.000000000000000000, 1.610000000000000098, -0.3440000000000000280 ) ) ;
#11651 = DIRECTION ( 'NONE',  ( 0.000000000000000000, 0.000000000000000000, -1.000000000000000000 ) ) ;
#11652 = ORIENTED_EDGE ( 'NONE', *, *, #12662, .F. ) ;
#11653 = DIRECTION ( 'NONE',  ( -1.000000000000000000, -0.000000000000000000, -0.000000000000000000 ) ) ;
#11654 = ORIENTED_EDGE ( 'NONE', *, *, #501, .F. ) ;
#11655 = EDGE_CURVE ( 'NONE', #6823, #4756, #4232, .T. ) ;
#11656 = DIRECTION ( 'NONE',  ( 0.000000000000000000, 0.000000000000000000, -1.000000000000000000 ) ) ;
#11657 = CYLINDRICAL_SURFACE ( 'NONE', #5468, 0.2624999999999997335 ) ;
#11658 = ORIENTED_EDGE ( 'NONE', *, *, #7147, .F. ) ;
#11659 = ADVANCED_FACE ( 'NONE', ( #15116 ), #9034, .F. ) ;
#11660 = CARTESIAN_POINT ( 'NONE',  ( 0.7727406610312560487, 0.1749999999999999889, -0.2070552360820117899 ) ) ;
#11661 = AXIS2_PLACEMENT_3D ( 'NONE', #5178, #7338, #14427 ) ;
#11662 = CARTESIAN_POINT ( 'NONE',  ( 1.131687341751868248, -0.4429445645322986902, -0.4840157155117131293 ) ) ;
#11663 = EDGE_CURVE ( 'NONE', #9095, #13629, #10015, .T. ) ;
#11664 = DIRECTION ( 'NONE',  ( 1.000000000000000000, 0.000000000000000000, 0.000000000000000000 ) ) ;
#11665 = VECTOR ( 'NONE', #4012, 39.37007874015748854 ) ;
#11666 = CARTESIAN_POINT ( 'NONE',  ( 7.144847001653046861E-17, -0.6334543218446814228, 0.000000000000000000 ) ) ;
#11667 = CARTESIAN_POINT ( 'NONE',  ( 3.566714410367414434, 1.985790321547726833, -0.6832061603422943108 ) ) ;
#11668 = VERTEX_POINT ( 'NONE', #2344 ) ;
#11669 = EDGE_CURVE ( 'NONE', #3133, #251, #10829, .T. ) ;
#11670 = CIRCLE ( 'NONE', #5567, 0.2625000000000000111 ) ;
#11671 = VERTEX_POINT ( 'NONE', #2572 ) ;
#11672 = DIRECTION ( 'NONE',  ( 1.000000000000000000, 0.000000000000000000, 0.000000000000000000 ) ) ;
#11673 = VERTEX_POINT ( 'NONE', #10532 ) ;
#11674 = EDGE_CURVE ( 'NONE', #9406, #3668, #2179, .T. ) ;
#11675 = CARTESIAN_POINT ( 'NONE',  ( 0.8999999999999998002, 0.1549999999999996103, -0.3799999999999999489 ) ) ;
#11676 = CARTESIAN_POINT ( 'NONE',  ( 0.8336852985356731915, -0.4829999999999998739, -0.4100337033397443709 ) ) ;
#11677 = DIRECTION ( 'NONE',  ( 0.000000000000000000, 0.000000000000000000, -1.000000000000000000 ) ) ;
#11678 = LINE ( 'NONE', #1183, #9245 ) ;
#11679 = ORIENTED_EDGE ( 'NONE', *, *, #365, .T. ) ;
#11680 = CARTESIAN_POINT ( 'NONE',  ( 0.000000000000000000, 0.000000000000000000, 0.000000000000000000 ) ) ;
#11681 = CIRCLE ( 'NONE', #14606, 2.500000000000000000 ) ;
#11682 = ADVANCED_FACE ( 'NONE', ( #4720 ), #8171, .T. ) ;
#11683 = CARTESIAN_POINT ( 'NONE',  ( 0.7513246802501661881, 2.561107494060246767E-17, -0.4293820849162032216 ) ) ;
#11684 = CARTESIAN_POINT ( 'NONE',  ( 3.875000000000000000, 1.059999999999999165, 0.000000000000000000 ) ) ;
#11685 = VECTOR ( 'NONE', #11541, 39.37007874015748143 ) ;
#11686 = EDGE_CURVE ( 'NONE', #651, #10168, #8335, .T. ) ;
#11687 = CARTESIAN_POINT ( 'NONE',  ( 1.522243911113194681, -0.3829999999999998961, -0.4784993797865369491 ) ) ;
#11688 = DIRECTION ( 'NONE',  ( 0.01412288512831213171, -3.675428035873183031E-19, -0.9999002670844990837 ) ) ;
#11689 = EDGE_CURVE ( 'NONE', #7182, #4577, #13902, .T. ) ;
#11690 = VECTOR ( 'NONE', #9234, 39.37007874015748143 ) ;
#11691 = CARTESIAN_POINT ( 'NONE',  ( 4.489587877062135135, 1.733016502558613725, -0.4335731954417103573 ) ) ;
#11692 = ORIENTED_EDGE ( 'NONE', *, *, #722, .T. ) ;
#11694 = ORIENTED_EDGE ( 'NONE', *, *, #11829, .T. ) ;
#11693 = DIRECTION ( 'NONE',  ( 0.000000000000000000, -4.591341165821852610E-16, 1.000000000000000000 ) ) ;
#11695 = ORIENTED_EDGE ( 'NONE', *, *, #4004, .T. ) ;
#11696 = FACE_OUTER_BOUND ( 'NONE', #7901, .T. ) ;
#11697 = ORIENTED_EDGE ( 'NONE', *, *, #10442, .T. ) ;
#11698 = LINE ( 'NONE', #8108, #4859 ) ;
#11699 = CARTESIAN_POINT ( 'NONE',  ( 3.875000000000000000, -0.9999999999999986677, 0.000000000000000000 ) ) ;
#11700 = FACE_BOUND ( 'NONE', #569, .T. ) ;
#11701 = ORIENTED_EDGE ( 'NONE', *, *, #3887, .T. ) ;
#11702 = CIRCLE ( 'NONE', #9743, 0.1899999999999996136 ) ;
#11703 = CARTESIAN_POINT ( 'NONE',  ( -0.01817859877509239372, 1.603284996591855194, -0.3809527529760087239 ) ) ;
#11704 = CARTESIAN_POINT ( 'NONE',  ( 0.6566154142300546503, -0.4311287871771214975, -0.4974659767684403433 ) ) ;
#11705 = AXIS2_PLACEMENT_3D ( 'NONE', #12169, #3770, #369 ) ;
#11706 = EDGE_CURVE ( 'NONE', #11919, #5059, #6843, .T. ) ;
#11707 = AXIS2_PLACEMENT_3D ( 'NONE', #15146, #1282, #3445 ) ;
#11708 = CARTESIAN_POINT ( 'NONE',  ( 0.8999999999999998002, 0.000000000000000000, -0.3799999999999999489 ) ) ;
#11709 = VECTOR ( 'NONE', #14088, 39.37007874015748143 ) ;
#11710 = DIRECTION ( 'NONE',  ( 0.000000000000000000, 0.000000000000000000, -1.000000000000000000 ) ) ;
#11711 = AXIS2_PLACEMENT_3D ( 'NONE', #7343, #11995, #6189 ) ;
#11712 = CIRCLE ( 'NONE', #8060, 0.1250000000000000278 ) ;
#11713 = LINE ( 'NONE', #4743, #9752 ) ;
#11714 = CARTESIAN_POINT ( 'NONE',  ( 0.6180000000000012150, 0.000000000000000000, 0.000000000000000000 ) ) ;
#11715 = EDGE_CURVE ( 'NONE', #4134, #3613, #2427, .T. ) ;
#11716 = CIRCLE ( 'NONE', #682, 0.6700292969071727223 ) ;
#11717 = CARTESIAN_POINT ( 'NONE',  ( 2.124999999999999556, -1.679378605318041950, 1.973878605318058810 ) ) ;
#11718 = DIRECTION ( 'NONE',  ( 0.000000000000000000, -1.000000000000000000, 0.000000000000000000 ) ) ;
#11719 = ORIENTED_EDGE ( 'NONE', *, *, #8692, .F. ) ;
#11720 = MECHANICAL_DESIGN_GEOMETRIC_PRESENTATION_REPRESENTATION (  '', ( #6345 ), #8547 ) ;
#11721 = DIRECTION ( 'NONE',  ( -1.000000000000000000, -0.000000000000000000, -0.000000000000000000 ) ) ;
#11723 = ORIENTED_EDGE ( 'NONE', *, *, #2600, .F. ) ;
#11722 = DIRECTION ( 'NONE',  ( 0.000000000000000000, 0.000000000000000000, 1.000000000000000000 ) ) ;
#11724 = VERTEX_POINT ( 'NONE', #9548 ) ;
#11725 = CIRCLE ( 'NONE', #7090, 0.07500000000000002498 ) ;
#11726 = CARTESIAN_POINT ( 'NONE',  ( 0.6500000000000001332, 3.654346048655703246E-16, -2.968000000000000860 ) ) ;
#11727 = DIRECTION ( 'NONE',  ( 0.000000000000000000, 0.000000000000000000, -1.000000000000000000 ) ) ;
#11728 = EDGE_LOOP ( 'NONE', ( #8943, #5784 ) ) ;
#11729 = CARTESIAN_POINT ( 'NONE',  ( 3.015109087180224771E-17, -0.4844395604395604904, 0.000000000000000000 ) ) ;
#11730 = CARTESIAN_POINT ( 'NONE',  ( 1.250000000000000000, -0.05999999999999986594, -0.4223386481965726857 ) ) ;
#11731 = DIRECTION ( 'NONE',  ( -1.000000000000000000, 0.000000000000000000, 0.000000000000000000 ) ) ;
#11732 = VECTOR ( 'NONE', #1761, 39.37007874015748143 ) ;
#11733 = ORIENTED_EDGE ( 'NONE', *, *, #7310, .T. ) ;
#11734 = EDGE_CURVE ( 'NONE', #6033, #10976, #5617, .T. ) ;
#11735 = CARTESIAN_POINT ( 'NONE',  ( 0.7040204553987591263, -0.3870671487057328886, 0.4900562082570797950 ) ) ;
#11736 = DIRECTION ( 'NONE',  ( 0.000000000000000000, 0.000000000000000000, -1.000000000000000000 ) ) ;
#11737 = DIRECTION ( 'NONE',  ( 0.000000000000000000, 0.000000000000000000, 1.000000000000000000 ) ) ;
#11738 = ORIENTED_EDGE ( 'NONE', *, *, #1279, .F. ) ;
#11739 = CARTESIAN_POINT ( 'NONE',  ( 0.000000000000000000, 1.559103846021539619, 0.000000000000000000 ) ) ;
#11740 = VERTEX_POINT ( 'NONE', #29 ) ;
#11741 = DIRECTION ( 'NONE',  ( 0.000000000000000000, 0.000000000000000000, 1.000000000000000000 ) ) ;
#11742 = ORIENTED_EDGE ( 'NONE', *, *, #4165, .F. ) ;
#11743 = CARTESIAN_POINT ( 'NONE',  ( -5.764454660286586870E-18, 0.1956296296296295978, 0.000000000000000000 ) ) ;
#11744 = VECTOR ( 'NONE', #342, 39.37007874015748854 ) ;
#11745 = CARTESIAN_POINT ( 'NONE',  ( 1.644431316733000026, -0.3408522091760272099, -0.4170406485181324396 ) ) ;
#11746 = CARTESIAN_POINT ( 'NONE',  ( 2.774999999999999911, 0.000000000000000000, 1.039370078740158965 ) ) ;
#11747 = CARTESIAN_POINT ( 'NONE',  ( 3.874999999999999556, 2.782000000000002693, 1.130000000000000560 ) ) ;
#11748 = ORIENTED_EDGE ( 'NONE', *, *, #5436, .T. ) ;
#11749 = ORIENTED_EDGE ( 'NONE', *, *, #9849, .F. ) ;
#11750 = CARTESIAN_POINT ( 'NONE',  ( 6.215861650065340527, 0.000000000000000000, 0.000000000000000000 ) ) ;
#11751 = LINE ( 'NONE', #1020, #3856 ) ;
#11752 = DIRECTION ( 'NONE',  ( 0.000000000000000000, 1.000000000000000000, -0.000000000000000000 ) ) ;
#11753 = CARTESIAN_POINT ( 'NONE',  ( 0.7372049720039718368, -0.0009098304392685509310, -0.4419334053338275226 ) ) ;
#11754 = VERTEX_POINT ( 'NONE', #5875 ) ;
#11755 = VECTOR ( 'NONE', #2577, 39.37007874015748143 ) ;
#11756 = CARTESIAN_POINT ( 'NONE',  ( 3.592530085043205368, 1.950116979243637028, -0.4132115743265128982 ) ) ;
#11757 = CARTESIAN_POINT ( 'NONE',  ( 1.558097216777236227, -0.02209972869556197164, 0.4779929771641632796 ) ) ;
#11758 = DIRECTION ( 'NONE',  ( 0.000000000000000000, 0.000000000000000000, 1.000000000000000000 ) ) ;
#11759 = EDGE_CURVE ( 'NONE', #7512, #11167, #6986, .T. ) ;
#11760 = ADVANCED_FACE ( 'NONE', ( #1487 ), #6170, .F. ) ;
#11761 = ADVANCED_FACE ( 'NONE', ( #12810 ), #3661, .T. ) ;
#11762 = DIRECTION ( 'NONE',  ( 0.000000000000000000, 1.000000000000000000, 0.000000000000000000 ) ) ;
#11763 = FACE_OUTER_BOUND ( 'NONE', #14174, .T. ) ;
#11764 = CIRCLE ( 'NONE', #11520, 2.960629921259841257 ) ;
#11765 = CARTESIAN_POINT ( 'NONE',  ( 4.605209778948695210, 1.806214611443159646, 0.1785906071940129292 ) ) ;
#11766 = ORIENTED_EDGE ( 'NONE', *, *, #11291, .F. ) ;
#11768 = EDGE_LOOP ( 'NONE', ( #13917, #14268, #9083, #7947 ) ) ;
#11767 = DIRECTION ( 'NONE',  ( -1.000000000000000000, -0.000000000000000000, -0.000000000000000000 ) ) ;
#11769 = EDGE_CURVE ( 'NONE', #7387, #1907, #10750, .T. ) ;
#11770 = EDGE_CURVE ( 'NONE', #4626, #7795, #14580, .T. ) ;
#11771 = CARTESIAN_POINT ( 'NONE',  ( 0.000000000000000000, 0.000000000000000000, 0.000000000000000000 ) ) ;
#11772 = ORIENTED_EDGE ( 'NONE', *, *, #10554, .T. ) ;
#11773 = DIRECTION ( 'NONE',  ( 0.000000000000000000, 0.000000000000000000, -1.000000000000000000 ) ) ;
#11774 =( NAMED_UNIT ( * ) PLANE_ANGLE_UNIT ( ) SI_UNIT ( $, .RADIAN. ) );
#11775 = FACE_OUTER_BOUND ( 'NONE', #4523, .T. ) ;
#11776 = ORIENTED_EDGE ( 'NONE', *, *, #12290, .F. ) ;
#11777 = LINE ( 'NONE', #11994, #12389 ) ;
#11778 = DIRECTION ( 'NONE',  ( 0.000000000000000000, -0.000000000000000000, -1.000000000000000000 ) ) ;
#11779 = CARTESIAN_POINT ( 'NONE',  ( 6.208491571325183145, 1.679378605318035733, -2.054378605318066153 ) ) ;
#11780 = CIRCLE ( 'NONE', #6397, 0.2944999999999987073 ) ;
#11781 = CARTESIAN_POINT ( 'NONE',  ( 3.426491571325181340, 2.360000000000015863, 0.9799999999999454703 ) ) ;
#11782 = CARTESIAN_POINT ( 'NONE',  ( 8.792093969802149189, 0.8799778768672790186, 6.829619984160658046E-17 ) ) ;
#11783 = DIRECTION ( 'NONE',  ( 1.000000000000000000, 0.000000000000000000, 0.000000000000000000 ) ) ;
#11784 = PLANE ( 'NONE',  #197 ) ;
#11785 = CARTESIAN_POINT ( 'NONE',  ( 4.585000156914120772, 1.718796672713930551, -0.3806726929799386094 ) ) ;
#11786 = ORIENTED_EDGE ( 'NONE', *, *, #2996, .F. ) ;
#11787 = DIRECTION ( 'NONE',  ( 1.000000000000000000, 0.000000000000000000, 0.000000000000000000 ) ) ;
#11789 = EDGE_LOOP ( 'NONE', ( #2032, #10515, #717, #8104 ) ) ;
#11788 = DIRECTION ( 'NONE',  ( -0.000000000000000000, -1.000000000000000000, -0.000000000000000000 ) ) ;
#11790 = ORIENTED_EDGE ( 'NONE', *, *, #6431, .F. ) ;
#11791 = ADVANCED_FACE ( 'NONE', ( #12200 ), #9992, .F. ) ;
#11792 = CARTESIAN_POINT ( 'NONE',  ( 3.426491571325181340, 0.000000000000000000, 1.000000000000000000 ) ) ;
#11793 = CARTESIAN_POINT ( 'NONE',  ( 0.3724999999999997757, -0.6590000000000000302, -0.3725000000000000533 ) ) ;
#11794 = CARTESIAN_POINT ( 'NONE',  ( 4.344846310392954436, 3.137999999999999901, 1.491010071662831171 ) ) ;
#11795 = ORIENTED_EDGE ( 'NONE', *, *, #46, .F. ) ;
#11796 = CARTESIAN_POINT ( 'NONE',  ( 0.7017867892446607581, -0.4844395604395603239, -0.4010711782184315233 ) ) ;
#11797 = ADVANCED_FACE ( 'NONE', ( #3875 ), #1780, .F. ) ;
#11798 = AXIS2_PLACEMENT_3D ( 'NONE', #3848, #5213, #10878 ) ;
#11799 = DIRECTION ( 'NONE',  ( 0.000000000000000000, 0.000000000000000000, -1.000000000000000000 ) ) ;
#11800 = DIRECTION ( 'NONE',  ( -0.9992912762382414327, -0.03489602031262312859, 0.01411428356268702201 ) ) ;
#11801 = ORIENTED_EDGE ( 'NONE', *, *, #13947, .F. ) ;
#11802 = CARTESIAN_POINT ( 'NONE',  ( 3.437516310781153273, 2.055659281767487023, -0.6089580415532643842 ) ) ;
#11803 = DIRECTION ( 'NONE',  ( 1.000000000000000000, 0.000000000000000000, 3.491481338843132961E-15 ) ) ;
#11804 = CARTESIAN_POINT ( 'NONE',  ( 2.775039370078740131, -1.679378605318047946, -2.054378605318054163 ) ) ;
#11805 = ORIENTED_EDGE ( 'NONE', *, *, #2870, .T. ) ;
#11806 = DIRECTION ( 'NONE',  ( 0.000000000000000000, 0.000000000000000000, -1.000000000000000000 ) ) ;
#11807 = ORIENTED_EDGE ( 'NONE', *, *, #5161, .T. ) ;
#11808 = AXIS2_PLACEMENT_3D ( 'NONE', #11338, #4393, #14938 ) ;
#11809 = LINE ( 'NONE', #8149, #1542 ) ;
#11810 = EDGE_LOOP ( 'NONE', ( #5064, #13651, #964, #1442 ) ) ;
#11811 = CARTESIAN_POINT ( 'NONE',  ( 2.774999999999999911, 0.9800000000000039790, 2.359999999999999876 ) ) ;
#11812 = ADVANCED_FACE ( 'NONE', ( #12268 ), #9534, .F. ) ;
#11813 = ADVANCED_FACE ( 'NONE', ( #12123 ), #12688, .F. ) ;
#11814 = CIRCLE ( 'NONE', #13792, 0.03999999999999998002 ) ;
#11815 = CARTESIAN_POINT ( 'NONE',  ( 2.124999999999999556, -2.360000000000000320, 1.575000000000016387 ) ) ;
#11816 = DIRECTION ( 'NONE',  ( 0.000000000000000000, 0.000000000000000000, -1.000000000000000000 ) ) ;
#11817 = LINE ( 'NONE', #7012, #14803 ) ;
#11818 = AXIS2_PLACEMENT_3D ( 'NONE', #11473, #972, #14284 ) ;
#11819 = ORIENTED_EDGE ( 'NONE', *, *, #15034, .F. ) ;
#11820 = ORIENTED_EDGE ( 'NONE', *, *, #9417, .F. ) ;
#11821 = EDGE_LOOP ( 'NONE', ( #3392, #211, #244, #7713 ) ) ;
#11822 = CIRCLE ( 'NONE', #13498, 1.502725933896874810 ) ;
#11823 = PRODUCT_DEFINITION_CONTEXT ( 'detailed design', #9200, 'design' ) ;
#11824 = CARTESIAN_POINT ( 'NONE',  ( 3.426491571325181784, 2.032298649151902392, 0.6051796186069025030 ) ) ;
#11825 = CLOSED_SHELL ( 'NONE', ( #2341, #10774, #1633, #10533, #10537, #5144, #13462, #7843, #2161, #7457, #2638, #3245, #7647, #939, #9528, #14403, #922, #9148, #743, #6044, #12481, #13173, #2593, #5588, #6895, #2721, #10097 ) ) ;
#11826 = CARTESIAN_POINT ( 'NONE',  ( 0.3208433835780706289, 1.603403919227001539, -0.2061884643224887181 ) ) ;
#11827 = CARTESIAN_POINT ( 'NONE',  ( 3.874999999999999556, 3.535499999999999421, 1.509999999999999787 ) ) ;
#11828 = EDGE_LOOP ( 'NONE', ( #711, #2089, #6276, #3865 ) ) ;
#11829 = EDGE_CURVE ( 'NONE', #1562, #14857, #3947, .T. ) ;
#11830 = CARTESIAN_POINT ( 'NONE',  ( 3.573766445277532622, 1.954426848217328594, -0.3997464416171771506 ) ) ;
#11831 = DIRECTION ( 'NONE',  ( -0.000000000000000000, -1.000000000000000000, -0.000000000000000000 ) ) ;
#11832 = CARTESIAN_POINT ( 'NONE',  ( 3.426491571325181340, 2.359999999999993214, -1.575000000000016831 ) ) ;
#11833 = AXIS2_PLACEMENT_3D ( 'NONE', #8562, #9632, #6118 ) ;
#11834 = CARTESIAN_POINT ( 'NONE',  ( 1.632672928280230362, 0.0005225660665716322373, -0.4769396479056465243 ) ) ;
#11835 = EDGE_LOOP ( 'NONE', ( #2504, #6253, #3010, #3374 ) ) ;
#11837 = ORIENTED_EDGE ( 'NONE', *, *, #171, .T. ) ;
#11836 = CARTESIAN_POINT ( 'NONE',  ( 0.4312750580175467308, 1.564824237736521351, 0.01491519342840733238 ) ) ;
#11838 = VECTOR ( 'NONE', #12340, 39.37007874015748143 ) ;
#11839 = VERTEX_POINT ( 'NONE', #13479 ) ;
#11840 = FACE_OUTER_BOUND ( 'NONE', #15138, .T. ) ;
#11841 = ORIENTED_EDGE ( 'NONE', *, *, #2797, .F. ) ;
#11842 = EDGE_CURVE ( 'NONE', #4719, #6847, #10983, .T. ) ;
#11843 = PRODUCT_DEFINITION_FORMATION_WITH_SPECIFIED_SOURCE ( 'ANY', '', #9961, .NOT_KNOWN. ) ;
#11844 = ADVANCED_FACE ( 'NONE', ( #12048 ), #1629, .F. ) ;
#11845 = FACE_BOUND ( 'NONE', #4466, .T. ) ;
#11846 = ORIENTED_EDGE ( 'NONE', *, *, #6878, .F. ) ;
#11847 = EDGE_CURVE ( 'NONE', #5675, #4181, #7533, .T. ) ;
#11848 = DIRECTION ( 'NONE',  ( -2.602462600580851747E-17, -1.000000000000000000, 0.000000000000000000 ) ) ;
#11849 = CARTESIAN_POINT ( 'NONE',  ( 3.874999999999999556, 2.750000000000000000, -1.320000000000000062 ) ) ;
#11850 = CARTESIAN_POINT ( 'NONE',  ( 3.544732980980179970, 1.997075164250705859, 0.6728923706171071606 ) ) ;
#11851 = LINE ( 'NONE', #7346, #9635 ) ;
#11852 = EDGE_CURVE ( 'NONE', #4913, #7544, #5860, .T. ) ;
#11853 = AXIS2_PLACEMENT_3D ( 'NONE', #7801, #4585, #4508 ) ;
#11854 = FACE_OUTER_BOUND ( 'NONE', #9596, .T. ) ;
#11855 = AXIS2_PLACEMENT_3D ( 'NONE', #3006, #2072, #7827 ) ;
#11856 = CARTESIAN_POINT ( 'NONE',  ( 0.7017867892446606470, 0.04143956043956045082, 0.4010711782184315233 ) ) ;
#11857 = CARTESIAN_POINT ( 'NONE',  ( 2.774999999999999911, -1.575000000000000178, 2.360000000000016751 ) ) ;
#11858 = CARTESIAN_POINT ( 'NONE',  ( 4.681089581896493712, 1.732453011165680401, 0.09841563256873263332 ) ) ;
#11859 = ORIENTED_EDGE ( 'NONE', *, *, #1499, .T. ) ;
#11860 = CARTESIAN_POINT ( 'NONE',  ( 0.6610344722576404486, -0.4494579783924679273, 0.4833528575413044148 ) ) ;
#11862 = ORIENTED_EDGE ( 'NONE', *, *, #8665, .T. ) ;
#11861 = FACE_BOUND ( 'NONE', #8, .T. ) ;
#11863 = ORIENTED_EDGE ( 'NONE', *, *, #236, .F. ) ;
#11864 = ADVANCED_FACE ( 'NONE', ( #705 ), #12433, .T. ) ;
#11865 = DIRECTION ( 'NONE',  ( -0.000000000000000000, 1.000000000000000000, -0.000000000000000000 ) ) ;
#11866 = CARTESIAN_POINT ( 'NONE',  ( 2.774999999999999911, 2.399999999999999911, -0.7000000000000007327 ) ) ;
#11867 = CARTESIAN_POINT ( 'NONE',  ( 2.824624536279283671, 0.5882431044538737330, 0.4601041732163942410 ) ) ;
#11868 = ORIENTED_EDGE ( 'NONE', *, *, #11377, .T. ) ;
#11869 = FACE_OUTER_BOUND ( 'NONE', #12013, .T. ) ;
#11870 = CIRCLE ( 'NONE', #5260, 2.960629921259841257 ) ;
#11871 = CONICAL_SURFACE ( 'NONE', #363, 0.4070000000000022489, 0.7853981633974547183 ) ;
#11872 = CARTESIAN_POINT ( 'NONE',  ( 2.124999999999999556, -0.9799999999999990941, -2.359999999999999876 ) ) ;
#11873 = LINE ( 'NONE', #14231, #6089 ) ;
#11874 = ADVANCED_FACE ( 'NONE', ( #1556 ), #13164, .F. ) ;
#11875 = ORIENTED_EDGE ( 'NONE', *, *, #8075, .F. ) ;
#11876 = AXIS2_PLACEMENT_3D ( 'NONE', #824, #5674, #4378 ) ;
#11877 = CARTESIAN_POINT ( 'NONE',  ( 0.6734872051250879732, -0.4131034743634533490, 0.4827143163826072003 ) ) ;
#11878 = CARTESIAN_POINT ( 'NONE',  ( 0.000000000000000000, 4.529999999999999361, 0.000000000000000000 ) ) ;
#11879 = AXIS2_PLACEMENT_3D ( 'NONE', #5702, #6860, #13349 ) ;
#11880 = DIRECTION ( 'NONE',  ( 0.000000000000000000, 0.000000000000000000, 1.000000000000000000 ) ) ;
#11881 = AXIS2_PLACEMENT_3D ( 'NONE', #4639, #2255, #10524 ) ;
#11882 = EDGE_LOOP ( 'NONE', ( #6647, #1145, #4621, #11071, #11354, #4985, #5554, #12772, #928 ) ) ;
#11883 = EDGE_CURVE ( 'NONE', #8572, #11419, #11472, .T. ) ;
#11884 = LINE ( 'NONE', #14239, #14544 ) ;
#11885 = EDGE_LOOP ( 'NONE', ( #11300, #6353, #13201, #7336 ) ) ;
#11886 = DIRECTION ( 'NONE',  ( 1.047444401652940007E-14, 0.000000000000000000, -1.000000000000000000 ) ) ;
#11887 = ORIENTED_EDGE ( 'NONE', *, *, #1822, .F. ) ;
#11888 = DIRECTION ( 'NONE',  ( -3.491481338843132961E-15, 0.000000000000000000, 1.000000000000000000 ) ) ;
#11889 = AXIS2_PLACEMENT_3D ( 'NONE', #2530, #281, #7209 ) ;
#11890 = CARTESIAN_POINT ( 'NONE',  ( 6.176491571325181340, -1.679378605318047946, -1.272378605318051248 ) ) ;
#11891 = DIRECTION ( 'NONE',  ( -1.000000000000000000, -0.000000000000000000, -0.000000000000000000 ) ) ;
#11892 = EDGE_CURVE ( 'NONE', #7601, #12557, #5550, .T. ) ;
#11893 = EDGE_CURVE ( 'NONE', #11318, #9755, #13639, .T. ) ;
#11894 = ORIENTED_EDGE ( 'NONE', *, *, #3103, .F. ) ;
#11895 = VERTEX_POINT ( 'NONE', #10288 ) ;
#11896 = ORIENTED_EDGE ( 'NONE', *, *, #11187, .T. ) ;
#11897 = DIRECTION ( 'NONE',  ( 0.000000000000000000, 0.000000000000000000, 1.000000000000000000 ) ) ;
#11898 = FACE_OUTER_BOUND ( 'NONE', #13962, .T. ) ;
#11899 = AXIS2_PLACEMENT_3D ( 'NONE', #9698, #9840, #4028 ) ;
#11900 = DIRECTION ( 'NONE',  ( 8.659560562354915602E-17, -0.7071067811865487940, 0.7071067811865462405 ) ) ;
#11901 = CARTESIAN_POINT ( 'NONE',  ( 0.8999999999999999112, -0.6429999999999999050, -0.3750000000000000555 ) ) ;
#11902 = VERTEX_POINT ( 'NONE', #13711 ) ;
#11903 = DIRECTION ( 'NONE',  ( -1.000000000000000000, -0.000000000000000000, -0.000000000000000000 ) ) ;
#11904 = CIRCLE ( 'NONE', #4080, 0.5000000000000001110 ) ;
#11905 = LINE ( 'NONE', #14036, #13642 ) ;
#11906 = DIRECTION ( 'NONE',  ( 0.000000000000000000, 0.000000000000000000, -1.000000000000000000 ) ) ;
#11907 = DIRECTION ( 'NONE',  ( 0.000000000000000000, -1.224646799147354933E-16, 1.000000000000000000 ) ) ;
#11908 = ADVANCED_FACE ( 'NONE', ( #851 ), #12560, .T. ) ;
#11909 = ORIENTED_EDGE ( 'NONE', *, *, #14769, .T. ) ;
#11911 = ORIENTED_EDGE ( 'NONE', *, *, #4610, .T. ) ;
#11910 = CARTESIAN_POINT ( 'NONE',  ( 6.826491571325181695, 1.272861240058668140E-16, 1.039370078740158965 ) ) ;
#11912 = VERTEX_POINT ( 'NONE', #10213 ) ;
#11913 = DIRECTION ( 'NONE',  ( -0.7071067811865450192, 0.000000000000000000, 0.7071067811865499042 ) ) ;
#11914 = VERTEX_POINT ( 'NONE', #12423 ) ;
#11915 = CARTESIAN_POINT ( 'NONE',  ( 3.874999999999999556, 3.137999999999999901, -1.320000000000000062 ) ) ;
#11916 = AXIS2_PLACEMENT_3D ( 'NONE', #1613, #10968, #7823 ) ;
#11917 = PRODUCT_CONTEXT ( 'NONE', #14363, 'mechanical' ) ;
#11918 = CARTESIAN_POINT ( 'NONE',  ( 0.8249999999999999556, -0.6429999999999999050, -0.3750000000000000555 ) ) ;
#11919 = VERTEX_POINT ( 'NONE', #1942 ) ;
#11920 = CARTESIAN_POINT ( 'NONE',  ( -0.07252880680210840869, 1.600831684639946184, -0.3809527529760086684 ) ) ;
#11921 = DIRECTION ( 'NONE',  ( -0.000000000000000000, -1.000000000000000000, -0.000000000000000000 ) ) ;
#11922 = AXIS2_PLACEMENT_3D ( 'NONE', #9353, #8506, #4836 ) ;
#11923 = DIRECTION ( 'NONE',  ( 0.000000000000000000, 0.000000000000000000, 1.000000000000000000 ) ) ;
#11924 = CONICAL_SURFACE ( 'NONE', #4606, 0.1899999999999996136, 0.7853981633974435050 ) ;
#11925 = ADVANCED_FACE ( 'NONE', ( #9220 ), #3323, .T. ) ;
#11926 = CARTESIAN_POINT ( 'NONE',  ( 0.3724999999999999423, -0.6589999999999996971, 0.3724999999999999423 ) ) ;
#11927 = AXIS2_PLACEMENT_3D ( 'NONE', #5203, #14603, #512 ) ;
#11928 = DIRECTION ( 'NONE',  ( 0.000000000000000000, -1.000000000000000000, 0.000000000000000000 ) ) ;
#11929 = CARTESIAN_POINT ( 'NONE',  ( 3.546155925590385838, 1.898807144323297003, 0.7421470037383380847 ) ) ;
#11930 = CARTESIAN_POINT ( 'NONE',  ( 3.874999999999999556, 3.567999999999999616, -1.542500000000000204 ) ) ;
#11931 = ORIENTED_EDGE ( 'NONE', *, *, #3432, .F. ) ;
#11932 = CARTESIAN_POINT ( 'NONE',  ( 0.6179999999999965521, 1.679378605318035733, -1.304378605318064821 ) ) ;
#11934 = ORIENTED_EDGE ( 'NONE', *, *, #4841, .T. ) ;
#11933 = DIRECTION ( 'NONE',  ( 0.000000000000000000, 0.000000000000000000, 1.000000000000000000 ) ) ;
#11935 = EDGE_LOOP ( 'NONE', ( #12273, #8334, #7985, #14955 ) ) ;
#11936 = CIRCLE ( 'NONE', #11705, 0.2944999999999987073 ) ;
#11937 = CIRCLE ( 'NONE', #3880, 0.7500000000000001110 ) ;
#11938 = DIRECTION ( 'NONE',  ( 0.000000000000000000, 0.000000000000000000, 1.000000000000000000 ) ) ;
#11939 = DIRECTION ( 'NONE',  ( 1.000000000000000000, 0.000000000000000000, -3.779312718515659280E-16 ) ) ;
#11940 = ORIENTED_EDGE ( 'NONE', *, *, #14843, .T. ) ;
#11941 = VECTOR ( 'NONE', #10879, 39.37007874015748143 ) ;
#11942 = DIRECTION ( 'NONE',  ( 0.000000000000000000, 1.000000000000000000, 0.000000000000000000 ) ) ;
#11943 = CONICAL_SURFACE ( 'NONE', #6100, 0.3750000000000004996, 0.7853981633974376209 ) ;
#11944 = DIRECTION ( 'NONE',  ( 0.000000000000000000, 1.000000000000000000, -2.708891287835076134E-14 ) ) ;
#11945 = VECTOR ( 'NONE', #12238, 39.37007874015748143 ) ;
#11946 = EDGE_CURVE ( 'NONE', #9348, #12293, #11725, .T. ) ;
#11947 = AXIS2_PLACEMENT_3D ( 'NONE', #7561, #7415, #3752 ) ;
#11948 = CARTESIAN_POINT ( 'NONE',  ( 0.6179999999999965521, -1.679378605318047946, -1.679378605318053497 ) ) ;
#11949 = EDGE_CURVE ( 'NONE', #5441, #1907, #4249, .T. ) ;
#11950 = ORIENTED_EDGE ( 'NONE', *, *, #2656, .T. ) ;
#11951 = EDGE_CURVE ( 'NONE', #3309, #5002, #12643, .T. ) ;
#11952 = CARTESIAN_POINT ( 'NONE',  ( 0.09500000000000431710, -1.679378605318047946, -1.679378605318053497 ) ) ;
#11953 = LINE ( 'NONE', #518, #11550 ) ;
#11954 = DIRECTION ( 'NONE',  ( -0.000000000000000000, -0.000000000000000000, 1.000000000000000000 ) ) ;
#11955 = EDGE_LOOP ( 'NONE', ( #10880, #4274, #9170, #4773 ) ) ;
#11956 = VECTOR ( 'NONE', #13203, 39.37007874015748143 ) ;
#11957 = AXIS2_PLACEMENT_3D ( 'NONE', #8617, #12201, #1860 ) ;
#11958 = DIRECTION ( 'NONE',  ( -1.000000000000000000, -0.000000000000000000, -0.000000000000000000 ) ) ;
#11959 = EDGE_LOOP ( 'NONE', ( #11041, #14180 ) ) ;
#11960 = EDGE_CURVE ( 'NONE', #14534, #3646, #3912, .T. ) ;
#11961 = CARTESIAN_POINT ( 'NONE',  ( -0.4349147617188414139, 1.559103846021539619, 0.008611041693274201769 ) ) ;
#11962 = VERTEX_POINT ( 'NONE', #2003 ) ;
#11963 = EDGE_CURVE ( 'NONE', #13670, #4509, #13556, .T. ) ;
#11964 = CARTESIAN_POINT ( 'NONE',  ( 2.002301348309084350, -0.1786631980423395716, -0.4121376268991520098 ) ) ;
#11965 = AXIS2_PLACEMENT_3D ( 'NONE', #8397, #318, #10765 ) ;
#11966 = CARTESIAN_POINT ( 'NONE',  ( 0.6179999999999962190, -1.679378605318048390, 1.679378605318054163 ) ) ;
#11967 = DIRECTION ( 'NONE',  ( -1.000000000000000000, -0.000000000000000000, -0.000000000000000000 ) ) ;
#11968 = CARTESIAN_POINT ( 'NONE',  ( 2.592367411162173063, 0.4049457270506677808, -0.4633846410852800468 ) ) ;
#11969 = VERTEX_POINT ( 'NONE', #14873 ) ;
#11970 = ORIENTED_EDGE ( 'NONE', *, *, #8020, .T. ) ;
#11971 = VERTEX_POINT ( 'NONE', #13780 ) ;
#11972 = EDGE_CURVE ( 'NONE', #9005, #13668, #709, .T. ) ;
#11973 = CIRCLE ( 'NONE', #1940, 0.1899999999999996136 ) ;
#11974 = CARTESIAN_POINT ( 'NONE',  ( 2.814370078740158210, 0.000000000000000000, 0.000000000000000000 ) ) ;
#11975 = DIRECTION ( 'NONE',  ( -1.000000000000000000, -0.000000000000000000, -0.000000000000000000 ) ) ;
#11976 = EDGE_CURVE ( 'NONE', #6847, #3928, #6359, .T. ) ;
#11977 = B_SPLINE_CURVE_WITH_KNOTS ( 'NONE', 3,
 ( #14221, #8500, #9647, #6132, #1443, #11860, #10712, #7493, #8573, #3908, #4910, #12995, #13212, #2607 ),
 .UNSPECIFIED., .F., .F.,
 ( 4, 2, 2, 2, 2, 2, 4 ),
 ( 0.000000000000000000, 0.001176052134299115362, 0.002352104268598230723, 0.002940130335747791115, 0.003528156402897351940, 0.004116182470046913199, 0.004704208537196473590 ),
 .UNSPECIFIED. ) ;
#11978 = CARTESIAN_POINT ( 'NONE',  ( 2.774999999999999911, 0.9799999999999438050, -2.360000000000016307 ) ) ;
#11979 = CARTESIAN_POINT ( 'NONE',  ( 2.775039370078740131, 1.679378605318035733, -1.679378605318065487 ) ) ;
#11980 = CARTESIAN_POINT ( 'NONE',  ( 3.875000000000000444, 1.884022191776434152, -0.5000000000000002220 ) ) ;
#11981 = EDGE_CURVE ( 'NONE', #5075, #11671, #8268, .T. ) ;
#11982 = CARTESIAN_POINT ( 'NONE',  ( 0.5400755080658357077, 0.1749999999999999889, -1.532626322880899838 ) ) ;
#11983 =( NAMED_UNIT ( * ) PLANE_ANGLE_UNIT ( ) SI_UNIT ( $, .RADIAN. ) );
#11984 = EDGE_LOOP ( 'NONE', ( #2117, #8254 ) ) ;
#11986 = ORIENTED_EDGE ( 'NONE', *, *, #1481, .T. ) ;
#11985 = CARTESIAN_POINT ( 'NONE',  ( 0.000000000000000000, 1.159999999999999698, 0.000000000000000000 ) ) ;
#11987 = EDGE_LOOP ( 'NONE', ( #10093, #1786, #12415, #10001 ) ) ;
#11988 = PRESENTATION_LAYER_ASSIGNMENT (  '', '', ( #7130 ) ) ;
#11989 = CARTESIAN_POINT ( 'NONE',  ( 5.567023771132172172, 0.000000000000000000, 0.000000000000000000 ) ) ;
#11990 = CARTESIAN_POINT ( 'NONE',  ( 3.426491571325181340, 1.679378605318042395, -1.416878605318058870 ) ) ;
#11991 = APPLICATION_PROTOCOL_DEFINITION ( 'draft international standard', 'automotive_design', 1998, #4500 ) ;
#11992 = CARTESIAN_POINT ( 'NONE',  ( 2.279764930208930007, 0.5637746725391985514, 0.4072339235668807067 ) ) ;
#11993 = ORIENTED_EDGE ( 'NONE', *, *, #5030, .T. ) ;
#11994 = CARTESIAN_POINT ( 'NONE',  ( 3.426491571325181340, -2.360000000000021636, -1.574999999999999734 ) ) ;
#11995 = DIRECTION ( 'NONE',  ( -0.000000000000000000, -1.000000000000000000, -0.000000000000000000 ) ) ;
#11996 = EDGE_CURVE ( 'NONE', #3733, #12843, #7162, .T. ) ;
#11997 = CARTESIAN_POINT ( 'NONE',  ( 2.156999999999999584, 1.679378605318042395, -1.416878605318059314 ) ) ;
#11998 = DIRECTION ( 'NONE',  ( -1.000000000000000000, -0.000000000000000000, -0.000000000000000000 ) ) ;
#11999 = AXIS2_PLACEMENT_3D ( 'NONE', #7913, #2009, #856 ) ;
#12000 = CARTESIAN_POINT ( 'NONE',  ( 2.774999999999999911, -1.679378605318041950, 1.679378605318059048 ) ) ;
#12001 = B_SPLINE_CURVE_WITH_KNOTS ( 'NONE', 3,
 ( #12399, #13618, #10480, #10047, #13903, #13536, #14704, #3081, #6604, #1920 ),
 .UNSPECIFIED., .F., .F.,
 ( 4, 2, 2, 2, 4 ),
 ( 0.07367938960722780761, 0.07700688573806144244, 0.08033438186889507726, 0.08366187799972872596, 0.08698937413056236079 ),
 .UNSPECIFIED. ) ;
#12002 = CARTESIAN_POINT ( 'NONE',  ( 0.8671983899133194340, -0.4446438992933860468, -0.4431244221569915487 ) ) ;
#12003 = CARTESIAN_POINT ( 'NONE',  ( 3.400138847590578273, 1.967011420863446824, 0.6697528156307519520 ) ) ;
#12005 = ORIENTED_EDGE ( 'NONE', *, *, #13053, .F. ) ;
#12004 = DIRECTION ( 'NONE',  ( 1.000000000000000000, 0.000000000000000000, 0.000000000000000000 ) ) ;
#12006 = EDGE_LOOP ( 'NONE', ( #12498, #2268, #11062, #5644 ) ) ;
#12007 = DIRECTION ( 'NONE',  ( 0.000000000000000000, -0.7071067811865350272, -0.7071067811865600072 ) ) ;
#12009 = ORIENTED_EDGE ( 'NONE', *, *, #6617, .F. ) ;
#12008 = FACE_BOUND ( 'NONE', #5514, .T. ) ;
#12010 = ORIENTED_EDGE ( 'NONE', *, *, #1117, .F. ) ;
#12011 = CARTESIAN_POINT ( 'NONE',  ( 0.7017867892446606470, 0.04143956043956045082, 0.4010711782184315233 ) ) ;
#12012 = CARTESIAN_POINT ( 'NONE',  ( 3.388933043275772494, 0.7513023213622327390, 0.4521337140780258279 ) ) ;
#12013 = EDGE_LOOP ( 'NONE', ( #7471, #3738, #15077, #10043 ) ) ;
#12014 = AXIS2_PLACEMENT_3D ( 'NONE', #8612, #13110, #7531 ) ;
#12015 = CARTESIAN_POINT ( 'NONE',  ( 6.208491571325183145, -1.679378605318047946, -2.054378605318054163 ) ) ;
#12016 = EDGE_CURVE ( 'NONE', #12243, #11081, #2930, .T. ) ;
#12017 = CARTESIAN_POINT ( 'NONE',  ( 0.6866570596051649877, 0.03904768965436217903, 0.4282026755330212708 ) ) ;
#12018 = FACE_OUTER_BOUND ( 'NONE', #11768, .T. ) ;
#12019 = ORIENTED_EDGE ( 'NONE', *, *, #13476, .T. ) ;
#12020 = CARTESIAN_POINT ( 'NONE',  ( 2.124999999999999556, 0.9800000000000039790, 2.359999999999999876 ) ) ;
#12021 = AXIS2_PLACEMENT_3D ( 'NONE', #4268, #12581, #792 ) ;
#12022 = CYLINDRICAL_SURFACE ( 'NONE', #3968, 2.500000000000000000 ) ;
#12023 = CARTESIAN_POINT ( 'NONE',  ( 3.426491571325181340, -1.679378605318041950, 1.941878605318059003 ) ) ;
#12024 = PRODUCT ( 'Inlet Housing', 'Inlet Housing', '', ( #13268 ) ) ;
#12025 = DIRECTION ( 'NONE',  ( -1.000000000000000000, -0.000000000000000000, -0.000000000000000000 ) ) ;
#12026 = ORIENTED_EDGE ( 'NONE', *, *, #8692, .T. ) ;
#12027 = CARTESIAN_POINT ( 'NONE',  ( -0.4150689297652816467, 1.581084130983675617, 0.04298503095531345380 ) ) ;
#12028 = VERTEX_POINT ( 'NONE', #3780 ) ;
#12029 = ADVANCED_FACE ( 'NONE', ( #162 ), #8327, .T. ) ;
#12030 = LINE ( 'NONE', #1539, #7088 ) ;
#12031 = EDGE_CURVE ( 'NONE', #2297, #4101, #9376, .T. ) ;
#12032 = EDGE_CURVE ( 'NONE', #9649, #4870, #4779, .T. ) ;
#12033 = LINE ( 'NONE', #14402, #1696 ) ;
#12034 = CARTESIAN_POINT ( 'NONE',  ( 3.874999999999999556, 3.567999999999999616, 1.542500000000000204 ) ) ;
#12035 = CIRCLE ( 'NONE', #1524, 0.2944999999999845519 ) ;
#12036 = DIRECTION ( 'NONE',  ( -0.000000000000000000, -1.000000000000000000, -0.000000000000000000 ) ) ;
#12037 = VECTOR ( 'NONE', #3039, 39.37007874015748854 ) ;
#12038 = ADVANCED_FACE ( 'NONE', ( #5929 ), #991, .T. ) ;
#12039 = DIRECTION ( 'NONE',  ( -0.000000000000000000, -1.000000000000000000, -0.000000000000000000 ) ) ;
#12040 = AXIS2_PLACEMENT_3D ( 'NONE', #8747, #4166, #2857 ) ;
#12041 = EDGE_LOOP ( 'NONE', ( #3026, #12736, #2224, #13560 ) ) ;
#12042 = ORIENTED_EDGE ( 'NONE', *, *, #3207, .F. ) ;
#12043 = EDGE_LOOP ( 'NONE', ( #10797, #575, #1665, #1295 ) ) ;
#12044 = CARTESIAN_POINT ( 'NONE',  ( 2.061999999999999833, 0.000000000000000000, 0.000000000000000000 ) ) ;
#12045 = CARTESIAN_POINT ( 'NONE',  ( 2.774999999999999911, -0.9799999999999986500, -3.359999999999999876 ) ) ;
#12046 = LINE ( 'NONE', #1626, #8602 ) ;
#12047 = FACE_OUTER_BOUND ( 'NONE', #1887, .T. ) ;
#12048 = FACE_OUTER_BOUND ( 'NONE', #11789, .T. ) ;
#12049 = CARTESIAN_POINT ( 'NONE',  ( 2.033926451083719833, 0.2322360065625572456, 0.4712722252671790457 ) ) ;
#12050 = CARTESIAN_POINT ( 'NONE',  ( 3.875000000000000000, 3.137999999999999901, 0.000000000000000000 ) ) ;
#12051 = AXIS2_PLACEMENT_3D ( 'NONE', #11150, #9167, #12446 ) ;
#12052 = ADVANCED_FACE ( 'NONE', ( #85 ), #11227, .T. ) ;
#12053 = CIRCLE ( 'NONE', #4986, 2.500000000000000444 ) ;
#12054 = AXIS2_PLACEMENT_3D ( 'NONE', #9269, #7050, #9421 ) ;
#12055 = ORIENTED_EDGE ( 'NONE', *, *, #9784, .F. ) ;
#12056 = ORIENTED_EDGE ( 'NONE', *, *, #4086, .T. ) ;
#12057 = ADVANCED_FACE ( 'NONE', ( #7234 ), #14895, .T. ) ;
#12058 = ORIENTED_EDGE ( 'NONE', *, *, #11591, .F. ) ;
#12059 = CARTESIAN_POINT ( 'NONE',  ( 0.1444440947987239432, 1.589814529920261954, 0.3809527529760087239 ) ) ;
#12060 = DIRECTION ( 'NONE',  ( -1.000000000000000000, -0.000000000000000000, -0.000000000000000000 ) ) ;
#12061 = DIRECTION ( 'NONE',  ( 0.4999999999999998335, 0.000000000000000000, 0.8660254037844388186 ) ) ;
#12062 = APPLICATION_PROTOCOL_DEFINITION ( 'draft international standard', 'automotive_design', 1998, #2650 ) ;
#12063 = CARTESIAN_POINT ( 'NONE',  ( 3.083590687937821428, 0.9932358216845013077, 0.4564464592100380136 ) ) ;
#12064 = VERTEX_POINT ( 'NONE', #1391 ) ;
#12065 = DIRECTION ( 'NONE',  ( 1.000000000000000000, 0.000000000000000000, 0.000000000000000000 ) ) ;
#12066 = CARTESIAN_POINT ( 'NONE',  ( 3.426491571325181340, 2.426945040795776443, 0.5999481385559803925 ) ) ;
#12067 = AXIS2_PLACEMENT_3D ( 'NONE', #9258, #12828, #13896 ) ;
#12068 = DIRECTION ( 'NONE',  ( 1.000000000000000000, 0.000000000000000000, 0.000000000000000000 ) ) ;
#12069 = CARTESIAN_POINT ( 'NONE',  ( 0.000000000000000000, 1.591999999999999638, 0.000000000000000000 ) ) ;
#12070 = DIRECTION ( 'NONE',  ( -1.000000000000000000, 0.000000000000000000, 0.000000000000000000 ) ) ;
#12071 = CIRCLE ( 'NONE', #10607, 1.812500000000000222 ) ;
#12072 = CARTESIAN_POINT ( 'NONE',  ( 3.521351135077507521, 2.009251905947152306, 0.6613697195036538634 ) ) ;
#12073 = DIRECTION ( 'NONE',  ( 1.000000000000000000, 0.000000000000000000, 0.000000000000000000 ) ) ;
#12074 = EDGE_CURVE ( 'NONE', #12552, #14802, #237, .T. ) ;
#12075 = ORIENTED_EDGE ( 'NONE', *, *, #6468, .F. ) ;
#12076 = LINE ( 'NONE', #14442, #9918 ) ;
#12078 = ORIENTED_EDGE ( 'NONE', *, *, #13935, .F. ) ;
#12077 = DIRECTION ( 'NONE',  ( 0.000000000000000000, 0.000000000000000000, -1.000000000000000000 ) ) ;
#12079 = ORIENTED_EDGE ( 'NONE', *, *, #1081, .F. ) ;
#12080 = FACE_OUTER_BOUND ( 'NONE', #9401, .T. ) ;
#12081 = DIRECTION ( 'NONE',  ( 0.000000000000000000, -1.000000000000000000, -0.000000000000000000 ) ) ;
#12082 = EDGE_LOOP ( 'NONE', ( #12673, #14709, #155, #5844, #6650, #7158, #2177, #6120, #12703, #5993, #2548, #15030 ) ) ;
#12083 = CYLINDRICAL_SURFACE ( 'NONE', #6320, 0.7500000000000001110 ) ;
#12084 = AXIS2_PLACEMENT_3D ( 'NONE', #5063, #13442, #3053 ) ;
#12085 = AXIS2_PLACEMENT_3D ( 'NONE', #14936, #1993, #4392 ) ;
#12086 = CIRCLE ( 'NONE', #4775, 0.2220000000000021678 ) ;
#12087 = CARTESIAN_POINT ( 'NONE',  ( 0.7070095302584743502, -0.01882438353555513505, 0.4738366780029916736 ) ) ;
#12088 = B_SPLINE_CURVE_WITH_KNOTS ( 'NONE', 3,
 ( #8093, #7853, #9080, #9009, #14889, #11447, #6704, #14731, #3259, #10300, #14809, #3191, #5713, #13723 ),
 .UNSPECIFIED., .F., .F.,
 ( 4, 2, 2, 2, 2, 2, 4 ),
 ( 1.734723475976807094E-18, 0.0004702396892684933098, 0.0007053595339027388805, 0.0009404793785369844512, 0.001175599223171230022, 0.001410719067805475593, 0.001880958757073978010 ),
 .UNSPECIFIED. ) ;
#12089 = DIRECTION ( 'NONE',  ( 0.000000000000000000, 0.000000000000000000, 1.000000000000000000 ) ) ;
#12090 = ORIENTED_EDGE ( 'NONE', *, *, #1822, .T. ) ;
#12091 = DIRECTION ( 'NONE',  ( 0.000000000000000000, -0.7071067811865487940, -0.7071067811865462405 ) ) ;
#12092 = CARTESIAN_POINT ( 'NONE',  ( 6.794491571325179891, -1.679378605318047946, -2.054378605318054163 ) ) ;
#12093 = LINE ( 'NONE', #7510, #2909 ) ;
#12094 = VERTEX_POINT ( 'NONE', #9886 ) ;
#12095 = AXIS2_PLACEMENT_3D ( 'NONE', #117, #1347, #1201 ) ;
#12096 = CYLINDRICAL_SURFACE ( 'NONE', #13555, 0.5000000000000001110 ) ;
#12097 = EDGE_CURVE ( 'NONE', #13668, #13702, #382, .T. ) ;
#12098 = ORIENTED_EDGE ( 'NONE', *, *, #11655, .T. ) ;
#12099 = CIRCLE ( 'NONE', #2817, 0.03999999999999998002 ) ;
#12100 = CARTESIAN_POINT ( 'NONE',  ( 1.831696981322114670, 0.1157067236523830062, 0.4136843993219122551 ) ) ;
#12101 = EDGE_LOOP ( 'NONE', ( #2705, #883, #1383, #8408 ) ) ;
#12102 = FACE_OUTER_BOUND ( 'NONE', #6777, .T. ) ;
#12103 = VECTOR ( 'NONE', #2704, 39.37007874015748854 ) ;
#12104 = CARTESIAN_POINT ( 'NONE',  ( 1.262572881824611803, -0.4300086559495954752, 0.4821670496917128679 ) ) ;
#12105 = CARTESIAN_POINT ( 'NONE',  ( -0.2249147617188422821, 1.559103846021539619, -0.3723417112827360209 ) ) ;
#12106 = CARTESIAN_POINT ( 'NONE',  ( 6.123233995736763571E-17, 0.000000000000000000, 0.4999999999999997224 ) ) ;
#12107 = CIRCLE ( 'NONE', #13086, 0.2219999999999999751 ) ;
#12108 = AXIS2_PLACEMENT_3D ( 'NONE', #7322, #14477, #14559 ) ;
#12109 = DIRECTION ( 'NONE',  ( 0.000000000000000000, 1.000000000000000000, 0.000000000000000000 ) ) ;
#12110 = EDGE_CURVE ( 'NONE', #6131, #4759, #459, .T. ) ;
#12111 = CARTESIAN_POINT ( 'NONE',  ( 3.874999999999999556, 3.137999999999999901, -1.320000000000000062 ) ) ;
#12112 = ORIENTED_EDGE ( 'NONE', *, *, #174, .F. ) ;
#12113 = ORIENTED_EDGE ( 'NONE', *, *, #3480, .F. ) ;
#12114 = VERTEX_POINT ( 'NONE', #11105 ) ;
#12115 = CONICAL_SURFACE ( 'NONE', #10172, 0.06999999999999829969, 0.7853981633974298493 ) ;
#12116 = CARTESIAN_POINT ( 'NONE',  ( 0.4125000000000000333, 0.1749999999999999889, -0.3724999999999999978 ) ) ;
#12117 = DIRECTION ( 'NONE',  ( 0.000000000000000000, 0.7071067811865612285, -0.7071067811865336949 ) ) ;
#12118 = AXIS2_PLACEMENT_3D ( 'NONE', #7092, #13943, #9305 ) ;
#12119 = AXIS2_PLACEMENT_3D ( 'NONE', #5545, #12556, #10058 ) ;
#12120 = DIRECTION ( 'NONE',  ( -1.047444401652940007E-14, 0.000000000000000000, 1.000000000000000000 ) ) ;
#12121 = ADVANCED_FACE ( 'NONE', ( #301 ), #9764, .F. ) ;
#12122 = DIRECTION ( 'NONE',  ( 0.000000000000000000, 0.000000000000000000, 1.000000000000000000 ) ) ;
#12123 = FACE_OUTER_BOUND ( 'NONE', #12041, .T. ) ;
#12124 = DIRECTION ( 'NONE',  ( 0.000000000000000000, 0.000000000000000000, -1.000000000000000000 ) ) ;
#12125 = CARTESIAN_POINT ( 'NONE',  ( 4.247991639008878550, 1.782319238603491174, -0.6520378312758601247 ) ) ;
#12126 = AXIS2_PLACEMENT_3D ( 'NONE', #7796, #731, #6649 ) ;
#12127 = EDGE_CURVE ( 'NONE', #10000, #3132, #7663, .T. ) ;
#12128 = EDGE_CURVE ( 'NONE', #5697, #3188, #4160, .T. ) ;
#12129 = AXIS2_PLACEMENT_3D ( 'NONE', #14575, #8695, #3956 ) ;
#12130 = CARTESIAN_POINT ( 'NONE',  ( 4.508361655903602383, 1.711445479664179592, -0.4931022144224059822 ) ) ;
#12131 = ORIENTED_EDGE ( 'NONE', *, *, #12366, .T. ) ;
#12132 = VERTEX_POINT ( 'NONE', #5082 ) ;
#12133 = EDGE_LOOP ( 'NONE', ( #14663, #2702, #5043, #7169 ) ) ;
#12134 = CARTESIAN_POINT ( 'NONE',  ( 0.007908111413600218964, -0.2214999999999999469, 0.5598942880828960966 ) ) ;
#12135 = CARTESIAN_POINT ( 'NONE',  ( 3.426491571325181340, 1.679378605318042395, -1.679378605318058604 ) ) ;
#12136 = DIRECTION ( 'NONE',  ( 0.000000000000000000, 0.000000000000000000, 1.000000000000000000 ) ) ;
#12137 = ADVANCED_FACE ( 'NONE', ( #7379 ), #7814, .F. ) ;
#12138 = TOROIDAL_SURFACE ( 'NONE', #10195, 0.7173254825712083171, 0.05999999999999999778 ) ;
#12139 = PRODUCT_CONTEXT ( 'NONE', #1558, 'mechanical' ) ;
#12140 = DIRECTION ( 'NONE',  ( 0.000000000000000000, -4.591341165822195764E-16, -1.000000000000000000 ) ) ;
#12141 = ORIENTED_EDGE ( 'NONE', *, *, #10238, .T. ) ;
#12142 = DIRECTION ( 'NONE',  ( -1.000000000000000000, -0.000000000000000000, -0.000000000000000000 ) ) ;
#12143 = CARTESIAN_POINT ( 'NONE',  ( -0.4125000000000000333, -0.6290000000000005587, 0.3724999999999999423 ) ) ;
#12144 = EDGE_CURVE ( 'NONE', #4756, #3922, #5010, .T. ) ;
#12145 = CARTESIAN_POINT ( 'NONE',  ( 2.449076186954514686E-17, -0.4430000000000000049, 0.000000000000000000 ) ) ;
#12146 = PRODUCT_DEFINITION_SHAPE ( 'NONE', 'NONE',  #15156 ) ;
#12147 = DIRECTION ( 'NONE',  ( 1.000000000000000000, 0.000000000000000000, 0.000000000000000000 ) ) ;
#12148 = LINE ( 'NONE', #204, #773 ) ;
#12149 = CARTESIAN_POINT ( 'NONE',  ( 3.441224298305551432, 1.974937406882123714, 0.6122973898694716866 ) ) ;
#12151 = VERTEX_POINT ( 'NONE', #2851 ) ;
#12150 = DIRECTION ( 'NONE',  ( 0.000000000000000000, 0.000000000000000000, 1.000000000000000000 ) ) ;
#12152 = ORIENTED_EDGE ( 'NONE', *, *, #14359, .T. ) ;
#12153 = CARTESIAN_POINT ( 'NONE',  ( 3.426491571325181340, 1.963962403007655677, 0.6625976281079839492 ) ) ;
#12155 = ORIENTED_EDGE ( 'NONE', *, *, #9984, .T. ) ;
#12154 = DIRECTION ( 'NONE',  ( -1.000000000000000000, -0.000000000000000000, -0.000000000000000000 ) ) ;
#12156 = ORIENTED_EDGE ( 'NONE', *, *, #5955, .F. ) ;
#12157 = ADVANCED_FACE ( 'NONE', ( #12102 ), #3995, .F. ) ;
#12158 = FACE_OUTER_BOUND ( 'NONE', #777, .T. ) ;
#12159 = FACE_OUTER_BOUND ( 'NONE', #2331, .T. ) ;
#12160 = ORIENTED_EDGE ( 'NONE', *, *, #601, .F. ) ;
#12161 = LINE ( 'NONE', #11015, #3075 ) ;
#12162 = CARTESIAN_POINT ( 'NONE',  ( 2.774999999999999911, 2.360000000000015863, 1.574999999999999956 ) ) ;
#12163 = EDGE_CURVE ( 'NONE', #14925, #1229, #5629, .T. ) ;
#12164 = CARTESIAN_POINT ( 'NONE',  ( 0.6922886459387326274, 0.0009147467600669257660, 0.4416098182902893909 ) ) ;
#12165 = CARTESIAN_POINT ( 'NONE',  ( 0.007386697474241961034, -0.2214999999999999469, 0.5229781811763314359 ) ) ;
#12166 = AXIS2_PLACEMENT_3D ( 'NONE', #357, #656, #3913 ) ;
#12167 = ORIENTED_EDGE ( 'NONE', *, *, #14457, .T. ) ;
#12168 = DIRECTION ( 'NONE',  ( 1.000000000000000000, 0.000000000000000000, 0.000000000000000000 ) ) ;
#12169 = CARTESIAN_POINT ( 'NONE',  ( 2.774999999999999911, 1.679378605318059048, 1.679378605318041506 ) ) ;
#12170 = DIRECTION ( 'NONE',  ( 1.000000000000000000, 0.000000000000000000, 0.000000000000000000 ) ) ;
#12171 = AXIS2_PLACEMENT_3D ( 'NONE', #12187, #9604, #14327 ) ;
#12172 = ORIENTED_EDGE ( 'NONE', *, *, #308, .T. ) ;
#12173 = CIRCLE ( 'NONE', #12652, 1.000000000000000444 ) ;
#12174 = AXIS2_PLACEMENT_3D ( 'NONE', #1486, #5095, #9827 ) ;
#12175 = CARTESIAN_POINT ( 'NONE',  ( 0.6179999999999965521, -1.679378605318047946, -1.679378605318053497 ) ) ;
#12176 = EDGE_LOOP ( 'NONE', ( #14302, #10205, #3502, #8732 ) ) ;
#12177 = AXIS2_PLACEMENT_3D ( 'NONE', #13154, #4840, #7145 ) ;
#12178 = CARTESIAN_POINT ( 'NONE',  ( 0.000000000000000000, 1.000000000000000000, 0.000000000000000000 ) ) ;
#12179 = ORIENTED_EDGE ( 'NONE', *, *, #1262, .F. ) ;
#12180 = PRESENTATION_STYLE_ASSIGNMENT (( #11259 ) ) ;
#12181 = CIRCLE ( 'NONE', #5841, 1.000000000000000666 ) ;
#12182 = DIRECTION ( 'NONE',  ( 0.000000000000000000, 0.000000000000000000, -1.000000000000000000 ) ) ;
#12183 = AXIS2_PLACEMENT_3D ( 'NONE', #11952, #8654, #13373 ) ;
#12184 = EDGE_CURVE ( 'NONE', #5449, #14644, #1695, .T. ) ;
#12185 = CARTESIAN_POINT ( 'NONE',  ( 0.8329939018324243882, -0.4323038960628863281, -0.3410777879097737775 ) ) ;
#12186 = CIRCLE ( 'NONE', #10735, 1.000000000000000222 ) ;
#12187 = CARTESIAN_POINT ( 'NONE',  ( 0.5400755080658357077, 0.1749999999999999889, -1.532626322880899838 ) ) ;
#12188 = CONICAL_SURFACE ( 'NONE', #1180, 0.05500000000000146438, 0.7853981633974547183 ) ;
#12189 = CIRCLE ( 'NONE', #2915, 0.7849999999999969225 ) ;
#12190 = CARTESIAN_POINT ( 'NONE',  ( 6.787121492585022509, 0.000000000000000000, 3.000000000000000444 ) ) ;
#12191 = EDGE_LOOP ( 'NONE', ( #13812, #7770, #2384, #3232 ) ) ;
#12192 = ORIENTED_EDGE ( 'NONE', *, *, #9984, .F. ) ;
#12193 = VERTEX_POINT ( 'NONE', #6448 ) ;
#12194 = PLANE ( 'NONE',  #12108 ) ;
#12195 = ORIENTED_EDGE ( 'NONE', *, *, #7638, .T. ) ;
#12196 = AXIS2_PLACEMENT_3D ( 'NONE', #12773, #2144, #5679 ) ;
#12197 = DIRECTION ( 'NONE',  ( 0.000000000000000000, 0.000000000000000000, 1.000000000000000000 ) ) ;
#12198 = CARTESIAN_POINT ( 'NONE',  ( 3.394491571325180423, -1.679378605318059048, -1.679378605318041950 ) ) ;
#12199 = CIRCLE ( 'NONE', #12932, 0.2225000000000012523 ) ;
#12200 = FACE_OUTER_BOUND ( 'NONE', #6886, .T. ) ;
#12201 = DIRECTION ( 'NONE',  ( 1.000000000000000000, 0.000000000000000000, 0.000000000000000000 ) ) ;
#12202 = AXIS2_PLACEMENT_3D ( 'NONE', #9533, #10518, #2558 ) ;
#12203 = ORIENTED_EDGE ( 'NONE', *, *, #8218, .T. ) ;
#12204 = VERTEX_POINT ( 'NONE', #2710 ) ;
#12205 = ORIENTED_EDGE ( 'NONE', *, *, #12948, .F. ) ;
#12206 = CARTESIAN_POINT ( 'NONE',  ( 2.774999999999999911, 1.272861240058668140E-16, -1.039370078740158965 ) ) ;
#12207 = CARTESIAN_POINT ( 'NONE',  ( 0.000000000000000000, -1.002374524060224757E-18, 0.000000000000000000 ) ) ;
#12208 = CARTESIAN_POINT ( 'NONE',  ( 4.374151734133344682, 0.9995751005560787883, 0.03350973656221049174 ) ) ;
#12209 = ITEM_DEFINED_TRANSFORMATION ( 'NONE', 'NONE', #6696,  #8424 ) ;
#12210 = CARTESIAN_POINT ( 'NONE',  ( 3.471303878679313115, 1.057055486693972757, 0.4509702841988744715 ) ) ;
#12211 = VERTEX_POINT ( 'NONE', #9744 ) ;
#12212 = CARTESIAN_POINT ( 'NONE',  ( 3.426491571325181340, 2.058905028113295455, -0.2209981660730358233 ) ) ;
#12213 = CARTESIAN_POINT ( 'NONE',  ( 3.265716245508940574, 2.461786362941181139, 0.4361376382133447804 ) ) ;
#12214 = EDGE_CURVE ( 'NONE', #2380, #13228, #8554, .T. ) ;
#12215 = ADVANCED_BREP_SHAPE_REPRESENTATION ( '', ( #491, #8424 ), #12311 ) ;
#12216 = EDGE_CURVE ( 'NONE', #8675, #6443, #12033, .T. ) ;
#12217 = DIRECTION ( 'NONE',  ( 0.000000000000000000, 0.000000000000000000, 1.000000000000000000 ) ) ;
#12218 = EDGE_CURVE ( 'NONE', #14149, #7690, #4143, .T. ) ;
#12219 = CARTESIAN_POINT ( 'NONE',  ( 5.939536975864664694E-17, 1.109999999999999876, 0.4850000000000001532 ) ) ;
#12220 = CARTESIAN_POINT ( 'NONE',  ( 6.826491571325181695, 0.000000000000000000, 2.960629921259841257 ) ) ;
#12221 = EDGE_CURVE ( 'NONE', #7301, #14777, #8740, .T. ) ;
#12222 = CARTESIAN_POINT ( 'NONE',  ( 2.774999999999999911, -1.679378605318041950, 1.679378605318059048 ) ) ;
#12224 = ORIENTED_EDGE ( 'NONE', *, *, #7466, .F. ) ;
#12223 = DIRECTION ( 'NONE',  ( 0.000000000000000000, 0.000000000000000000, -1.000000000000000000 ) ) ;
#12225 = ORIENTED_EDGE ( 'NONE', *, *, #4180, .T. ) ;
#12226 = CARTESIAN_POINT ( 'NONE',  ( -0.2324059764400444317, 1.569496918332967228, -0.3593665467752061304 ) ) ;
#12228 = ORIENTED_EDGE ( 'NONE', *, *, #10072, .F. ) ;
#12227 = CARTESIAN_POINT ( 'NONE',  ( 5.567023771132172172, 0.000000000000000000, 1.500000000000000222 ) ) ;
#12229 = ORIENTED_EDGE ( 'NONE', *, *, #14265, .T. ) ;
#12230 = PLANE ( 'NONE',  #7768 ) ;
#12231 = FACE_OUTER_BOUND ( 'NONE', #1036, .T. ) ;
#12232 = ORIENTED_EDGE ( 'NONE', *, *, #9530, .T. ) ;
#12233 = DIRECTION ( 'NONE',  ( -1.000000000000000000, -0.000000000000000000, -0.000000000000000000 ) ) ;
#12234 = CARTESIAN_POINT ( 'NONE',  ( 0.4999999999999996114, 1.866025403784438819, -6.123233995736761105E-17 ) ) ;
#12235 = AXIS2_PLACEMENT_3D ( 'NONE', #5188, #274, #10854 ) ;
#12236 = DIMENSIONAL_EXPONENTS ( 1.000000000000000000, 0.000000000000000000, 0.000000000000000000, 0.000000000000000000, 0.000000000000000000, 0.000000000000000000, 0.000000000000000000 ) ;
#12237 = DIRECTION ( 'NONE',  ( -0.000000000000000000, -1.000000000000000000, -0.000000000000000000 ) ) ;
#12238 = DIRECTION ( 'NONE',  ( -0.7071067811865460184, 0.000000000000000000, 0.7071067811865490160 ) ) ;
#12239 = EDGE_LOOP ( 'NONE', ( #8161, #10510, #7825, #112 ) ) ;
#12240 = DIRECTION ( 'NONE',  ( 1.000000000000000000, 0.000000000000000000, 0.000000000000000000 ) ) ;
#12241 = DIRECTION ( 'NONE',  ( -1.000000000000000000, -0.000000000000000000, -0.000000000000000000 ) ) ;
#12242 = EDGE_CURVE ( 'NONE', #4263, #6919, #5222, .T. ) ;
#12243 = VERTEX_POINT ( 'NONE', #2778 ) ;
#12244 = CARTESIAN_POINT ( 'NONE',  ( 4.250664904820700585, 0.9439471567310199207, -0.3303580885322055516 ) ) ;
#12245 = CARTESIAN_POINT ( 'NONE',  ( 0.6180000000000012150, 0.000000000000000000, 0.000000000000000000 ) ) ;
#12246 = ORIENTED_EDGE ( 'NONE', *, *, #627, .F. ) ;
#12247 = ADVANCED_FACE ( 'NONE', ( #1612 ), #13174, .F. ) ;
#12248 = CARTESIAN_POINT ( 'NONE',  ( 0.7441558489118152986, 4.164134020615923019E-16, 0.4356293359425711387 ) ) ;
#12249 = ORIENTED_EDGE ( 'NONE', *, *, #14591, .F. ) ;
#12250 = CARTESIAN_POINT ( 'NONE',  ( 0.4125000000000000333, 0.000000000000000000, -0.4124999999999999778 ) ) ;
#12251 = CARTESIAN_POINT ( 'NONE',  ( 6.794491571325179891, -1.679378605318048390, 1.679378605318054163 ) ) ;
#12252 = CARTESIAN_POINT ( 'NONE',  ( 0.7815405595936760763, -0.4436696693102589184, -0.3492667155310359983 ) ) ;
#12253 = VECTOR ( 'NONE', #13764, 39.37007874015748854 ) ;
#12254 = LINE ( 'NONE', #4236, #6567 ) ;
#12255 = LINE ( 'NONE', #13178, #8197 ) ;
#12256 = CARTESIAN_POINT ( 'NONE',  ( 1.397260334976608398, 0.007251848866960407085, -0.4201477693899776100 ) ) ;
#12257 = DIRECTION ( 'NONE',  ( 0.000000000000000000, 0.000000000000000000, -1.000000000000000000 ) ) ;
#12258 = ORIENTED_EDGE ( 'NONE', *, *, #11483, .T. ) ;
#12259 = VERTEX_POINT ( 'NONE', #2367 ) ;
#12260 = EDGE_LOOP ( 'NONE', ( #6495, #6162, #12930, #8288 ) ) ;
#12261 = EDGE_CURVE ( 'NONE', #1386, #9230, #1207, .T. ) ;
#12262 = EDGE_CURVE ( 'NONE', #7123, #10530, #956, .T. ) ;
#12263 = CARTESIAN_POINT ( 'NONE',  ( 8.849999999999999645, 0.9399413264884247665, 6.829619984160658046E-17 ) ) ;
#12264 = ORIENTED_EDGE ( 'NONE', *, *, #11018, .F. ) ;
#12265 = CARTESIAN_POINT ( 'NONE',  ( -0.4349147617188414694, 0.7512260236060024354, 0.008611041693274290240 ) ) ;
#12266 = CARTESIAN_POINT ( 'NONE',  ( 0.6735393331370975734, -0.4714463074374599660, -0.4543474816912257408 ) ) ;
#12267 = PRODUCT ( 'MAT-052', 'MAT-052', '', ( #11917 ) ) ;
#12268 = FACE_OUTER_BOUND ( 'NONE', #3049, .T. ) ;
#12269 = CARTESIAN_POINT ( 'NONE',  ( 3.944129661530210385, 1.867491090171841339, -0.4951980309903490363 ) ) ;
#12270 = VECTOR ( 'NONE', #4849, 39.37007874015748143 ) ;
#12271 = ORIENTED_EDGE ( 'NONE', *, *, #12869, .F. ) ;
#12272 = SPHERICAL_SURFACE ( 'NONE', #3711, 0.8499999999999999778 ) ;
#12273 = ORIENTED_EDGE ( 'NONE', *, *, #10706, .F. ) ;
#12274 = EDGE_LOOP ( 'NONE', ( #3418, #12386, #5583, #3566 ) ) ;
#12275 = PRODUCT_DEFINITION_CONTEXT ( 'detailed design', #3728, 'design' ) ;
#12276 = ORIENTED_EDGE ( 'NONE', *, *, #1965, .F. ) ;
#12277 = DIRECTION ( 'NONE',  ( 1.000000000000000000, 0.000000000000000000, 0.000000000000000000 ) ) ;
#12278 = EDGE_CURVE ( 'NONE', #12557, #616, #6596, .T. ) ;
#12279 = CARTESIAN_POINT ( 'NONE',  ( 2.124999999999999556, 0.7000000000000030642, 2.399999999999999911 ) ) ;
#12280 = FACE_OUTER_BOUND ( 'NONE', #13945, .T. ) ;
#12281 = DIRECTION ( 'NONE',  ( -0.8660254037844433705, 0.000000000000000000, -0.4999999999999920064 ) ) ;
#12282 = ORIENTED_EDGE ( 'NONE', *, *, #13411, .T. ) ;
#12283 = DIRECTION ( 'NONE',  ( 0.000000000000000000, 0.000000000000000000, -1.000000000000000000 ) ) ;
#12284 = CARTESIAN_POINT ( 'NONE',  ( 3.283006985701197866, 2.457536269194010359, 0.4593688321371918737 ) ) ;
#12285 = DIRECTION ( 'NONE',  ( -1.000000000000000000, -0.000000000000000000, -0.000000000000000000 ) ) ;
#12286 = VECTOR ( 'NONE', #8903, 39.37007874015748143 ) ;
#12287 = CARTESIAN_POINT ( 'NONE',  ( 8.840371647876674288, 0.8816637705348994158, 0.09817148304380068913 ) ) ;
#12288 = CARTESIAN_POINT ( 'NONE',  ( 0.9542757771954346602, -0.4472635993787555386, -0.4276257322837787034 ) ) ;
#12289 = CARTESIAN_POINT ( 'NONE',  ( 4.544485495091622695, 1.738146795016368262, 0.3429988673886200101 ) ) ;
#12290 = EDGE_CURVE ( 'NONE', #5059, #11919, #5867, .T. ) ;
#12292 = ORIENTED_EDGE ( 'NONE', *, *, #12402, .T. ) ;
#12291 = PLANE ( 'NONE',  #5704 ) ;
#12293 = VERTEX_POINT ( 'NONE', #7046 ) ;
#12294 = EDGE_CURVE ( 'NONE', #1313, #11668, #15063, .T. ) ;
#12295 = AXIS2_PLACEMENT_3D ( 'NONE', #10253, #10404, #12755 ) ;
#12296 = CARTESIAN_POINT ( 'NONE',  ( -0.3117416060218557994, 1.602949672542212989, -0.2219532054890435979 ) ) ;
#12298 = ORIENTED_EDGE ( 'NONE', *, *, #343, .T. ) ;
#12297 = CARTESIAN_POINT ( 'NONE',  ( 3.405153689607044232, 3.567999999999999616, 1.491010071662831171 ) ) ;
#12299 = EDGE_LOOP ( 'NONE', ( #12298, #1418, #10594, #7002 ) ) ;
#12300 = CARTESIAN_POINT ( 'NONE',  ( 0.6558056096843538629, -0.01866721106089168705, 0.5013356986195881548 ) ) ;
#12301 = LINE ( 'NONE', #435, #3555 ) ;
#12302 = VERTEX_POINT ( 'NONE', #4233 ) ;
#12303 = DIRECTION ( 'NONE',  ( 0.7071067811865460184, 8.659560562354951347E-17, 0.7071067811865490160 ) ) ;
#12304 = CARTESIAN_POINT ( 'NONE',  ( 2.156999999999999584, 1.679378605318059048, 1.679378605318041506 ) ) ;
#12305 = EDGE_CURVE ( 'NONE', #9581, #1151, #4305, .T. ) ;
#12306 = DIRECTION ( 'NONE',  ( 0.000000000000000000, 0.000000000000000000, -1.000000000000000000 ) ) ;
#12307 = APPLICATION_CONTEXT ( 'automotive_design' ) ;
#12308 = CARTESIAN_POINT ( 'NONE',  ( 6.826491571325181695, 1.679378605318035733, -1.272378605318063016 ) ) ;
#12309 = VECTOR ( 'NONE', #8123, 39.37007874015748143 ) ;
#12310 = DIRECTION ( 'NONE',  ( -0.000000000000000000, -1.000000000000000000, 0.000000000000000000 ) ) ;
#12311 =( GEOMETRIC_REPRESENTATION_CONTEXT ( 3 ) GLOBAL_UNCERTAINTY_ASSIGNED_CONTEXT ( ( #15031 ) ) GLOBAL_UNIT_ASSIGNED_CONTEXT ( ( #11158, #4051, #7871 ) ) REPRESENTATION_CONTEXT ( 'NONE', 'WORKASPACE' ) );
#12312 = EDGE_LOOP ( 'NONE', ( #14714, #5869 ) ) ;
#12313 = DIRECTION ( 'NONE',  ( -0.000000000000000000, -1.000000000000000000, -0.000000000000000000 ) ) ;
#12314 = CARTESIAN_POINT ( 'NONE',  ( 3.874999999999999556, 3.137999999999999901, 1.320000000000000062 ) ) ;
#12315 = EDGE_CURVE ( 'NONE', #1080, #9538, #11624, .T. ) ;
#12316 = CARTESIAN_POINT ( 'NONE',  ( 0.4349147617188415249, 0.7512260236060024354, 0.008611041693268213504 ) ) ;
#12317 = EDGE_CURVE ( 'NONE', #694, #12204, #11973, .T. ) ;
#12318 = CARTESIAN_POINT ( 'NONE',  ( 2.774999999999999911, 0.9800000000000039790, 3.360000000000000320 ) ) ;
#12319 = CARTESIAN_POINT ( 'NONE',  ( 2.045067168503163391, 0.3290769108334317683, -0.4105096428946750642 ) ) ;
#12320 = ORIENTED_EDGE ( 'NONE', *, *, #4050, .F. ) ;
#12321 = AXIS2_PLACEMENT_3D ( 'NONE', #359, #8579, #4209 ) ;
#12322 = CARTESIAN_POINT ( 'NONE',  ( 3.613973162031111741, 0.9969999999999999973, -0.3889491967554554730 ) ) ;
#12323 = ORIENTED_EDGE ( 'NONE', *, *, #7005, .F. ) ;
#12324 = DIRECTION ( 'NONE',  ( 0.000000000000000000, 9.641816448226552334E-15, 1.000000000000000000 ) ) ;
#12325 = EDGE_CURVE ( 'NONE', #10522, #436, #7744, .T. ) ;
#12326 =( NAMED_UNIT ( * ) SI_UNIT ( $, .STERADIAN. ) SOLID_ANGLE_UNIT ( ) );
#12327 = CARTESIAN_POINT ( 'NONE',  ( 0.8287146145289983057, -0.4323349699879636132, -0.3513609214607458231 ) ) ;
#12328 = CARTESIAN_POINT ( 'NONE',  ( 1.002134052359566097, -0.4429990928571921338, -0.4270146172744395674 ) ) ;
#12329 = EDGE_CURVE ( 'NONE', #11902, #10962, #11181, .T. ) ;
#12330 = ORIENTED_EDGE ( 'NONE', *, *, #14939, .T. ) ;
#12331 = CIRCLE ( 'NONE', #12897, 0.03999999999999998002 ) ;
#12332 = LINE ( 'NONE', #13699, #14287 ) ;
#12333 = CARTESIAN_POINT ( 'NONE',  ( 0.8374673721983860730, -0.4832242842617602840, -0.3334348852663109875 ) ) ;
#12334 = VECTOR ( 'NONE', #8298, 39.37007874015748143 ) ;
#12335 = CARTESIAN_POINT ( 'NONE',  ( 0.06299999999999994493, 1.679378605318035733, -1.272378605318059686 ) ) ;
#12336 = EDGE_LOOP ( 'NONE', ( #8545, #14765, #13360, #9291 ) ) ;
#12337 = EDGE_LOOP ( 'NONE', ( #11156, #11875, #8719, #7438 ) ) ;
#12338 = CARTESIAN_POINT ( 'NONE',  ( 0.7017867892446606470, -0.4844395604395603239, 0.4010711782184315233 ) ) ;
#12339 = ORIENTED_EDGE ( 'NONE', *, *, #6553, .T. ) ;
#12340 = DIRECTION ( 'NONE',  ( -0.000000000000000000, -1.000000000000000000, -0.000000000000000000 ) ) ;
#12341 = CARTESIAN_POINT ( 'NONE',  ( 0.9176380235743000213, 0.000000000000000000, -0.1164708448095589793 ) ) ;
#12342 = AXIS2_PLACEMENT_3D ( 'NONE', #8146, #11577, #2316 ) ;
#12343 = CARTESIAN_POINT ( 'NONE',  ( 3.426491571325181340, 1.954234464180151676, -0.6847610993685215863 ) ) ;
#12344 = AXIS2_PLACEMENT_3D ( 'NONE', #12457, #8112, #13821 ) ;
#12345 = CIRCLE ( 'NONE', #5763, 0.03999999999999997308 ) ;
#12346 = DIRECTION ( 'NONE',  ( 0.000000000000000000, 0.000000000000000000, 1.000000000000000000 ) ) ;
#12347 = ADVANCED_FACE ( 'NONE', ( #10553 ), #4591, .T. ) ;
#12348 = EDGE_CURVE ( 'NONE', #8207, #4719, #12001, .T. ) ;
#12349 = ORIENTED_EDGE ( 'NONE', *, *, #11759, .T. ) ;
#12350 = ORIENTED_EDGE ( 'NONE', *, *, #11401, .F. ) ;
#12351 = CIRCLE ( 'NONE', #13807, 2.499999999999999556 ) ;
#12352 = ORIENTED_EDGE ( 'NONE', *, *, #3269, .F. ) ;
#12353 = VECTOR ( 'NONE', #13250, 39.37007874015748143 ) ;
#12354 = ORIENTED_EDGE ( 'NONE', *, *, #12813, .F. ) ;
#12355 = CARTESIAN_POINT ( 'NONE',  ( 2.124999999999999556, -1.575000000000016387, -2.359999999999999876 ) ) ;
#12356 = CARTESIAN_POINT ( 'NONE',  ( -5.764454660286586870E-18, -0.2214999999999999469, 0.000000000000000000 ) ) ;
#12357 = CARTESIAN_POINT ( 'NONE',  ( 4.370923089943242523, 0.9979667740156152878, -0.06586474272559393606 ) ) ;
#12358 = CARTESIAN_POINT ( 'NONE',  ( 6.826491571325181695, -1.679378605318048390, 1.679378605318054163 ) ) ;
#12359 = ORIENTED_EDGE ( 'NONE', *, *, #13842, .T. ) ;
#12360 = LINE ( 'NONE', #639, #9958 ) ;
#12361 = DIRECTION ( 'NONE',  ( 0.000000000000000000, -1.000000000000000000, 0.000000000000000000 ) ) ;
#12362 = CONICAL_SURFACE ( 'NONE', #14814, 0.2624999999999997335, 0.7853981633974479459 ) ;
#12363 = DIRECTION ( 'NONE',  ( 0.000000000000000000, 0.000000000000000000, -1.000000000000000000 ) ) ;
#12364 = CARTESIAN_POINT ( 'NONE',  ( 4.769268701363833074, 3.567999999999999616, 0.3249191361593796734 ) ) ;
#12365 = ADVANCED_FACE ( 'NONE', ( #3512 ), #9339, .T. ) ;
#12366 = EDGE_CURVE ( 'NONE', #694, #6001, #5455, .T. ) ;
#12367 = CARTESIAN_POINT ( 'NONE',  ( 8.792093969803303821, 0.8799778768673193197, 0.04156183585338274478 ) ) ;
#12368 = CARTESIAN_POINT ( 'NONE',  ( 0.9577688866514744159, -0.4806004831388784870, -0.4232852336075703104 ) ) ;
#12369 = CARTESIAN_POINT ( 'NONE',  ( 4.351048328242368868, 1.728421760757865355, 0.5811182005463045863 ) ) ;
#12371 = ORIENTED_EDGE ( 'NONE', *, *, #9917, .F. ) ;
#12370 = CARTESIAN_POINT ( 'NONE',  ( 3.781939775458268205, 1.913296957465108861, -0.4918119683718932267 ) ) ;
#12372 = AXIS2_PLACEMENT_3D ( 'NONE', #9630, #406, #13264 ) ;
#12373 = B_SPLINE_CURVE_WITH_KNOTS ( 'NONE', 3,
 ( #693, #14712, #1931, #6112, #6178, #6613, #10836, #11340, #14940, #6683, #3173, #842, #11502, #4623 ),
 .UNSPECIFIED., .F., .F.,
 ( 4, 2, 2, 2, 2, 2, 4 ),
 ( 0.000000000000000000, 0.0003612929182778039307, 0.0007225858365556078614, 0.001083878754833411846, 0.001445171673111215723, 0.002167757509666824126, 0.002890343346222432747 ),
 .UNSPECIFIED. ) ;
#12374 = ORIENTED_EDGE ( 'NONE', *, *, #7664, .T. ) ;
#12376 = ORIENTED_EDGE ( 'NONE', *, *, #958, .F. ) ;
#12375 = DIRECTION ( 'NONE',  ( -0.7070715176384831935, -0.7070715176384805289, -0.009986885842351453380 ) ) ;
#12377 = VERTEX_POINT ( 'NONE', #3439 ) ;
#12378 = FACE_BOUND ( 'NONE', #11220, .T. ) ;
#12379 = DIRECTION ( 'NONE',  ( 0.000000000000000000, 0.000000000000000000, -1.000000000000000000 ) ) ;
#12380 = ORIENTED_EDGE ( 'NONE', *, *, #14106, .T. ) ;
#12381 = CARTESIAN_POINT ( 'NONE',  ( 6.826491571325181695, 0.000000000000000000, 0.000000000000000000 ) ) ;
#12382 = DIRECTION ( 'NONE',  ( 0.000000000000000000, 0.000000000000000000, -1.000000000000000000 ) ) ;
#12383 = CIRCLE ( 'NONE', #1147, 0.08500000000000004774 ) ;
#12384 = LINE ( 'NONE', #1899, #1567 ) ;
#12385 = CARTESIAN_POINT ( 'NONE',  ( 2.774999999999999911, 0.9799999999999436939, -3.360000000000016751 ) ) ;
#12386 = ORIENTED_EDGE ( 'NONE', *, *, #3641, .T. ) ;
#12387 = DIRECTION ( 'NONE',  ( 0.000000000000000000, 0.000000000000000000, -1.000000000000000000 ) ) ;
#12388 = CARTESIAN_POINT ( 'NONE',  ( 3.426585660050375903, 0.9751674090406495798, -0.2235762390674587985 ) ) ;
#12389 = VECTOR ( 'NONE', #47, 39.37007874015748143 ) ;
#12390 = CARTESIAN_POINT ( 'NONE',  ( 4.373886831741767622, 1.706962534117436592, -0.6224998300045747612 ) ) ;
#12391 = VERTEX_POINT ( 'NONE', #6892 ) ;
#12392 = PRODUCT ( 'Cap Screw', 'Cap Screw', '', ( #14278 ) ) ;
#12393 = CARTESIAN_POINT ( 'NONE',  ( 3.426491571325181340, -0.6999999999999587663, 2.400000000000012790 ) ) ;
#12394 = DIRECTION ( 'NONE',  ( 0.000000000000000000, 0.000000000000000000, -1.000000000000000000 ) ) ;
#12395 = ORIENTED_EDGE ( 'NONE', *, *, #260, .F. ) ;
#12396 = CARTESIAN_POINT ( 'NONE',  ( -0.2099999999999999922, 1.239999999999999991, -0.3809527529760087239 ) ) ;
#12397 = ORIENTED_EDGE ( 'NONE', *, *, #11014, .T. ) ;
#12398 = CIRCLE ( 'NONE', #9495, 0.3750000000000004996 ) ;
#12399 = CARTESIAN_POINT ( 'NONE',  ( 3.876560711617219823, 1.855806856933289506, -0.7500000000000001110 ) ) ;
#12400 = ADVANCED_FACE ( 'NONE', ( #8114 ), #5879, .F. ) ;
#12401 = CONICAL_SURFACE ( 'NONE', #1161, 0.2041999999999996596, 0.7853981633974460586 ) ;
#12402 = EDGE_CURVE ( 'NONE', #5284, #12094, #9778, .T. ) ;
#12403 = SURFACE_SIDE_STYLE ('',( #14341 ) ) ;
#12404 = CARTESIAN_POINT ( 'NONE',  ( 3.426491571325181340, 3.360000000000000320, -0.9800000000000012035 ) ) ;
#12405 = EDGE_CURVE ( 'NONE', #3309, #12028, #13672, .T. ) ;
#12406 = DIRECTION ( 'NONE',  ( 0.000000000000000000, -1.000000000000000000, 0.000000000000000000 ) ) ;
#12407 = VERTEX_POINT ( 'NONE', #3820 ) ;
#12408 = AXIS2_PLACEMENT_3D ( 'NONE', #12358, #11219, #716 ) ;
#12409 = CARTESIAN_POINT ( 'NONE',  ( 3.874999999999999556, 3.137999999999999901, -1.097499999999998810 ) ) ;
#12410 = CARTESIAN_POINT ( 'NONE',  ( 2.775039370078740131, -1.679378605318047946, -1.679378605318053497 ) ) ;
#12411 = AXIS2_PLACEMENT_3D ( 'NONE', #12687, #12525, #15141 ) ;
#12412 = ADVANCED_FACE ( 'NONE', ( #199 ), #8418, .F. ) ;
#12413 = DIRECTION ( 'NONE',  ( 1.000000000000000000, 0.000000000000000000, 0.000000000000000000 ) ) ;
#12414 = ORIENTED_EDGE ( 'NONE', *, *, #7230, .T. ) ;
#12415 = ORIENTED_EDGE ( 'NONE', *, *, #6160, .F. ) ;
#12416 = CARTESIAN_POINT ( 'NONE',  ( 0.000000000000000000, 1.503199999999999870, 0.000000000000000000 ) ) ;
#12417 = ORIENTED_EDGE ( 'NONE', *, *, #6560, .T. ) ;
#12418 = DIRECTION ( 'NONE',  ( -1.000000000000000000, -0.000000000000000000, -0.000000000000000000 ) ) ;
#12419 = VECTOR ( 'NONE', #2782, 39.37007874015748143 ) ;
#12420 = CIRCLE ( 'NONE', #10478, 0.5000000000000001110 ) ;
#12421 = CARTESIAN_POINT ( 'NONE',  ( 0.6729666568098592316, -0.4031619489883325191, -0.4872504569466303836 ) ) ;
#12422 = AXIS2_PLACEMENT_3D ( 'NONE', #10152, #950, #12501 ) ;
#12423 = CARTESIAN_POINT ( 'NONE',  ( 2.124999999999999556, 1.679378605318059048, 1.384878605318041744 ) ) ;
#12424 = VECTOR ( 'NONE', #7045, 39.37007874015748143 ) ;
#12425 = AXIS2_PLACEMENT_3D ( 'NONE', #11982, #102, #1488 ) ;
#12426 = CARTESIAN_POINT ( 'NONE',  ( 4.064979089242817700, 1.806308836204446822, 0.7263547114196443610 ) ) ;
#12427 = ORIENTED_EDGE ( 'NONE', *, *, #9575, .T. ) ;
#12428 = AXIS2_PLACEMENT_3D ( 'NONE', #8808, #2986, #11395 ) ;
#12429 = AXIS2_PLACEMENT_3D ( 'NONE', #1610, #9390, #8529 ) ;
#12430 = EDGE_LOOP ( 'NONE', ( #12819, #10604 ) ) ;
#12431 = ORIENTED_EDGE ( 'NONE', *, *, #11981, .F. ) ;
#12432 = EDGE_CURVE ( 'NONE', #7033, #14200, #11239, .T. ) ;
#12433 = CONICAL_SURFACE ( 'NONE', #13409, 2.960629921259841257, 0.7853981633974552734 ) ;
#12434 = VERTEX_POINT ( 'NONE', #11997 ) ;
#12435 = CARTESIAN_POINT ( 'NONE',  ( -0.3725000000000002198, 0.2159999999999999420, -0.3725000000000000533 ) ) ;
#12436 = DIRECTION ( 'NONE',  ( -1.000000000000000000, 0.000000000000000000, 0.000000000000000000 ) ) ;
#12437 = FACE_BOUND ( 'NONE', #5107, .T. ) ;
#12438 = ADVANCED_FACE ( 'NONE', ( #12916 ), #3678, .F. ) ;
#12439 = CARTESIAN_POINT ( 'NONE',  ( 4.665325695584414469E-17, 1.603403463250997918, 0.3809527529760087239 ) ) ;
#12440 = EDGE_LOOP ( 'NONE', ( #12417, #1728, #13263, #2317 ) ) ;
#12441 = CARTESIAN_POINT ( 'NONE',  ( 3.390179639970223313, 0.6913388717410868800, 0.3921396980529558429 ) ) ;
#12442 = CARTESIAN_POINT ( 'NONE',  ( 2.774999999999999911, -1.575000000000027489, -1.574999999999989297 ) ) ;
#12443 = DIRECTION ( 'NONE',  ( 6.483702463810914196E-14, 0.000000000000000000, -1.000000000000000000 ) ) ;
#12444 = CARTESIAN_POINT ( 'NONE',  ( 3.394491571325183088, 1.679378605318059048, 1.679378605318041506 ) ) ;
#12445 = CARTESIAN_POINT ( 'NONE',  ( 4.529882331337859114, 1.713284349967738818, 0.4645268969338811615 ) ) ;
#12447 = ORIENTED_EDGE ( 'NONE', *, *, #7095, .T. ) ;
#12446 = DIRECTION ( 'NONE',  ( 0.000000000000000000, 0.000000000000000000, -1.000000000000000000 ) ) ;
#12448 = ORIENTED_EDGE ( 'NONE', *, *, #11282, .F. ) ;
#12450 = ORIENTED_EDGE ( 'NONE', *, *, #3468, .F. ) ;
#12449 = CARTESIAN_POINT ( 'NONE',  ( 0.09500000000000431710, 1.679378605318035733, -1.679378605318065487 ) ) ;
#12451 = VERTEX_POINT ( 'NONE', #11779 ) ;
#12452 = AXIS2_PLACEMENT_3D ( 'NONE', #12835, #14434, #3896 ) ;
#12453 = CARTESIAN_POINT ( 'NONE',  ( 0.7406097974541305806, 0.1956296296296295978, 0.000000000000000000 ) ) ;
#12454 = EDGE_CURVE ( 'NONE', #9031, #12926, #15150, .T. ) ;
#12455 = CARTESIAN_POINT ( 'NONE',  ( 0.8999999999999999112, -0.4829999999999998739, -0.3750000000000000555 ) ) ;
#12456 = ORIENTED_EDGE ( 'NONE', *, *, #7011, .F. ) ;
#12457 = CARTESIAN_POINT ( 'NONE',  ( 0.8999999999999999112, -0.4429999999999998939, -0.3750000000000000555 ) ) ;
#12458 = CARTESIAN_POINT ( 'NONE',  ( 3.874999999999999556, 3.137999999999999901, 1.320000000000000062 ) ) ;
#12459 = DIRECTION ( 'NONE',  ( -1.000000000000000000, -0.000000000000000000, -0.000000000000000000 ) ) ;
#12460 = CARTESIAN_POINT ( 'NONE',  ( 2.977166378293599980, 0.8979166429007079397, -0.4579496274252315979 ) ) ;
#12461 = CARTESIAN_POINT ( 'NONE',  ( 1.010163005730224883, -0.4429751326668778244, -0.4086419528574875004 ) ) ;
#12462 = VERTEX_POINT ( 'NONE', #13132 ) ;
#12463 = DIRECTION ( 'NONE',  ( -1.000000000000000000, -0.000000000000000000, -0.000000000000000000 ) ) ;
#12464 = DIRECTION ( 'NONE',  ( 0.7071067811865496822, 0.000000000000000000, -0.7071067811865452413 ) ) ;
#12465 = CARTESIAN_POINT ( 'NONE',  ( 0.1807106342563528367, 1.379999999999999671, 5.178337979384803075E-18 ) ) ;
#12466 = DIRECTION ( 'NONE',  ( 0.000000000000000000, 0.000000000000000000, 1.000000000000000000 ) ) ;
#12467 = VERTEX_POINT ( 'NONE', #1505 ) ;
#12468 = CARTESIAN_POINT ( 'NONE',  ( 2.094146026541975510E-17, -1.002374524060224757E-18, -0.1520000000000001905 ) ) ;
#12469 = ORIENTED_EDGE ( 'NONE', *, *, #14979, .T. ) ;
#12470 = EDGE_CURVE ( 'NONE', #14804, #7417, #8276, .T. ) ;
#12471 = CARTESIAN_POINT ( 'NONE',  ( 0.7349234941866550352, -0.4417196455735734606, -0.4440226803674550138 ) ) ;
#12472 = FACE_OUTER_BOUND ( 'NONE', #10051, .T. ) ;
#12473 = CARTESIAN_POINT ( 'NONE',  ( 2.774999999999999911, -2.360000000000016751, -0.9799999999999431388 ) ) ;
#12474 = ORIENTED_EDGE ( 'NONE', *, *, #15000, .F. ) ;
#12475 = CARTESIAN_POINT ( 'NONE',  ( 3.426491571325181340, 0.9800000000000039790, 3.360000000000000320 ) ) ;
#12476 = AXIS2_PLACEMENT_3D ( 'NONE', #12946, #1463, #13090 ) ;
#12477 = CARTESIAN_POINT ( 'NONE',  ( 3.464728362965293851, 1.935613442860778299, 0.7069208286046223533 ) ) ;
#12478 = LINE ( 'NONE', #9296, #10588 ) ;
#12479 = ORIENTED_EDGE ( 'NONE', *, *, #5208, .F. ) ;
#12480 = ORIENTED_EDGE ( 'NONE', *, *, #6452, .F. ) ;
#12481 = ADVANCED_FACE ( 'NONE', ( #7127 ), #7270, .F. ) ;
#12482 = EDGE_CURVE ( 'NONE', #8673, #6629, #1946, .T. ) ;
#12483 = DIRECTION ( 'NONE',  ( 0.000000000000000000, 1.000000000000000000, 0.000000000000000000 ) ) ;
#12484 = VERTEX_POINT ( 'NONE', #6190 ) ;
#12485 = EDGE_CURVE ( 'NONE', #12941, #4204, #10517, .T. ) ;
#12486 = CARTESIAN_POINT ( 'NONE',  ( 2.980731298636167370, 2.750000000000000000, 0.3249191361593797844 ) ) ;
#12487 = CARTESIAN_POINT ( 'NONE',  ( 3.405153689607044232, 3.567999999999999616, -1.491010071662831171 ) ) ;
#12488 = VECTOR ( 'NONE', #13708, 39.37007874015748143 ) ;
#12489 = DIRECTION ( 'NONE',  ( -1.000000000000000000, 0.000000000000000000, 0.000000000000000000 ) ) ;
#12490 = EDGE_CURVE ( 'NONE', #11602, #2942, #5121, .T. ) ;
#12491 = LINE ( 'NONE', #3325, #14849 ) ;
#12492 = EDGE_LOOP ( 'NONE', ( #763, #13890, #2300, #5540 ) ) ;
#12493 = CARTESIAN_POINT ( 'NONE',  ( 4.152466769471746311, 1.791617367317514864, -0.6983344528546440166 ) ) ;
#12494 = ORIENTED_EDGE ( 'NONE', *, *, #14617, .F. ) ;
#12495 = EDGE_CURVE ( 'NONE', #13702, #7063, #2742, .T. ) ;
#12496 = ORIENTED_EDGE ( 'NONE', *, *, #2125, .F. ) ;
#12497 = B_SPLINE_CURVE_WITH_KNOTS ( 'NONE', 3,
 ( #13456, #12537, #2924, #1830, #6516, #6667, #11325, #3072, #4223, #11172, #7737, #11402, #823, #10113 ),
 .UNSPECIFIED., .F., .F.,
 ( 4, 2, 2, 2, 2, 2, 4 ),
 ( 0.000000000000000000, 0.0007185039784459185813, 0.001437007956891837163, 0.001796259946114796020, 0.002155511935337754877, 0.002514763924560713734, 0.002874015913783673024 ),
 .UNSPECIFIED. ) ;
#12498 = ORIENTED_EDGE ( 'NONE', *, *, #5767, .F. ) ;
#12499 = LINE ( 'NONE', #2018, #9223 ) ;
#12500 = DIRECTION ( 'NONE',  ( 1.000000000000000000, 0.000000000000000000, 0.000000000000000000 ) ) ;
#12501 = DIRECTION ( 'NONE',  ( -0.7071067811865441310, 0.7071067811865509034, 0.000000000000000000 ) ) ;
#12502 = FACE_OUTER_BOUND ( 'NONE', #12979, .T. ) ;
#12503 =( REPRESENTATION_RELATIONSHIP ('NONE','NONE', #3591, #10912 ) REPRESENTATION_RELATIONSHIP_WITH_TRANSFORMATION ( #5333 )SHAPE_REPRESENTATION_RELATIONSHIP( ) );
#12504 = VERTEX_POINT ( 'NONE', #2519 ) ;
#12505 = CARTESIAN_POINT ( 'NONE',  ( 3.876560711617219379, 1.855806856933289950, 0.7500000000000001110 ) ) ;
#12506 = AXIS2_PLACEMENT_3D ( 'NONE', #11878, #2237, #11803 ) ;
#12507 = DIRECTION ( 'NONE',  ( -1.000000000000000000, -0.000000000000000000, -0.000000000000000000 ) ) ;
#12508 = EDGE_CURVE ( 'NONE', #13413, #10132, #9708, .T. ) ;
#12509 = CIRCLE ( 'NONE', #13241, 0.4070000000000022489 ) ;
#12510 = CARTESIAN_POINT ( 'NONE',  ( 0.9618999659839394534, -0.4466846464728802535, -0.4182560267626411754 ) ) ;
#12511 = EDGE_CURVE ( 'NONE', #6601, #11615, #2523, .T. ) ;
#12512 = CARTESIAN_POINT ( 'NONE',  ( 4.380579497543963363, 1.706994051371499177, 0.6171253673838056342 ) ) ;
#12514 = EDGE_LOOP ( 'NONE', ( #13001, #14445, #13836, #9373 ) ) ;
#12513 = CARTESIAN_POINT ( 'NONE',  ( 3.538134827540111438, 2.007021158475892797, -0.3702066563325129289 ) ) ;
#12515 = ORIENTED_EDGE ( 'NONE', *, *, #414, .F. ) ;
#12517 = ORIENTED_EDGE ( 'NONE', *, *, #13239, .F. ) ;
#12516 = DIRECTION ( 'NONE',  ( 0.7071067811865376918, 0.000000000000000000, -0.7071067811865573427 ) ) ;
#12518 =( BOUNDED_CURVE ( )  B_SPLINE_CURVE ( 3, ( #7881, #6436, #1902, #6592 ),
 .UNSPECIFIED., .F., .F. ) 
 B_SPLINE_CURVE_WITH_KNOTS ( ( 4, 4 ),
 ( 3.926990816987247168, 4.677482395344810584 ),
 .UNSPECIFIED. ) 
 CURVE ( )  GEOMETRIC_REPRESENTATION_ITEM ( )  RATIONAL_B_SPLINE_CURVE ( ( 1.000000000000000000, 0.9536117119880161974, 0.9536117119880161974, 1.000000000000000000 ) ) 
 REPRESENTATION_ITEM ( '' )  );
#12519 = ORIENTED_EDGE ( 'NONE', *, *, #11513, .F. ) ;
#12520 = DIRECTION ( 'NONE',  ( -0.01412288512831213171, 3.675428035873182550E-19, 0.9999002670844991947 ) ) ;
#12521 = DIRECTION ( 'NONE',  ( 1.000000000000000000, 0.000000000000000000, 0.000000000000000000 ) ) ;
#12522 = ORIENTED_EDGE ( 'NONE', *, *, #2469, .T. ) ;
#12523 = CIRCLE ( 'NONE', #14740, 0.1899999999999996136 ) ;
#12524 = CARTESIAN_POINT ( 'NONE',  ( 6.176491571325181340, -1.679378605318047946, -1.679378605318053497 ) ) ;
#12525 = DIRECTION ( 'NONE',  ( 1.000000000000000000, 0.000000000000000000, -1.224646799147353207E-16 ) ) ;
#12526 = CARTESIAN_POINT ( 'NONE',  ( 2.187203820042824542, 0.4712135623730921985, 0.5000000000000000000 ) ) ;
#12527 = FACE_OUTER_BOUND ( 'NONE', #13364, .T. ) ;
#12528 = CARTESIAN_POINT ( 'NONE',  ( 0.8999999999999998002, 0.01999999999999975409, -0.3799999999999999489 ) ) ;
#12529 = EDGE_CURVE ( 'NONE', #2516, #9310, #5257, .T. ) ;
#12530 = ORIENTED_EDGE ( 'NONE', *, *, #8510, .F. ) ;
#12531 = EDGE_CURVE ( 'NONE', #5110, #3609, #5109, .T. ) ;
#12532 = CYLINDRICAL_SURFACE ( 'NONE', #13865, 0.3803340137431718282 ) ;
#12533 = VECTOR ( 'NONE', #14234, 39.37007874015748143 ) ;
#12534 = CARTESIAN_POINT ( 'NONE',  ( 3.392241908693700125, 0.9914823872279339145, 0.1312138895577312503 ) ) ;
#12535 = CARTESIAN_POINT ( 'NONE',  ( 3.694525655941882203, 1.838693524946998004, -0.7841639951857555246 ) ) ;
#12536 = CIRCLE ( 'NONE', #8162, 0.1520000000000001905 ) ;
#12537 = CARTESIAN_POINT ( 'NONE',  ( 0.7441595030246626052, -0.4430000000000003935, 0.4356261515797149042 ) ) ;
#12539 = ORIENTED_EDGE ( 'NONE', *, *, #14843, .F. ) ;
#12538 = DIRECTION ( 'NONE',  ( -1.000000000000000000, 0.000000000000000000, 0.000000000000000000 ) ) ;
#12540 = ORIENTED_EDGE ( 'NONE', *, *, #6907, .F. ) ;
#12541 = CARTESIAN_POINT ( 'NONE',  ( 3.426491571325181340, -1.679378605318059048, -1.973878605318027724 ) ) ;
#12542 = DIRECTION ( 'NONE',  ( 0.000000000000000000, 0.000000000000000000, -1.000000000000000000 ) ) ;
#12543 = CARTESIAN_POINT ( 'NONE',  ( 1.625945750338193108, -0.2839166429008007642, 0.4770346645432458343 ) ) ;
#12544 = CARTESIAN_POINT ( 'NONE',  ( 0.7241094260644779235, -0.4377363598224605634, -0.4546250289486069018 ) ) ;
#12545 = CARTESIAN_POINT ( 'NONE',  ( 2.774999999999999911, -0.9799999999999986500, -3.359999999999999876 ) ) ;
#12546 = DIRECTION ( 'NONE',  ( 0.000000000000000000, -0.000000000000000000, 1.000000000000000000 ) ) ;
#12547 = ORIENTED_EDGE ( 'NONE', *, *, #12325, .F. ) ;
#12548 = CARTESIAN_POINT ( 'NONE',  ( 6.826491571325181695, 1.679378605318035733, -1.679378605318065487 ) ) ;
#12549 = DIRECTION ( 'NONE',  ( -1.000000000000000000, -0.000000000000000000, -0.000000000000000000 ) ) ;
#12550 = CIRCLE ( 'NONE', #14506, 0.4349999999999999423 ) ;
#12551 = DIRECTION ( 'NONE',  ( 0.000000000000000000, 0.000000000000000000, 1.000000000000000000 ) ) ;
#12552 = VERTEX_POINT ( 'NONE', #1878 ) ;
#12553 = DIRECTION ( 'NONE',  ( 0.000000000000000000, 0.000000000000000000, 1.000000000000000000 ) ) ;
#12554 = LINE ( 'NONE', #2078, #10364 ) ;
#12555 = PRODUCT_DEFINITION_FORMATION_WITH_SPECIFIED_SOURCE ( 'ANY', '', #12024, .NOT_KNOWN. ) ;
#12556 = DIRECTION ( 'NONE',  ( -0.000000000000000000, 1.000000000000000000, 1.224646799147353207E-16 ) ) ;
#12557 = VERTEX_POINT ( 'NONE', #6410 ) ;
#12558 = DIRECTION ( 'NONE',  ( -0.9781476007338071321, 0.000000000000000000, 0.2079116908177521816 ) ) ;
#12559 = CARTESIAN_POINT ( 'NONE',  ( 0.7117500205947747682, -0.4296287437428823464, -0.4679153652930406193 ) ) ;
#12560 = CYLINDRICAL_SURFACE ( 'NONE', #3168, 0.07500000000000002498 ) ;
#12561 = VECTOR ( 'NONE', #11939, 39.37007874015748143 ) ;
#12562 = CARTESIAN_POINT ( 'NONE',  ( 3.475703039784956871, 2.035382413711712246, 0.3018570397846632170 ) ) ;
#12563 = EDGE_CURVE ( 'NONE', #1935, #2080, #14738, .T. ) ;
#12564 = AXIS2_PLACEMENT_3D ( 'NONE', #14635, #12039, #462 ) ;
#12565 = AXIS2_PLACEMENT_3D ( 'NONE', #5986, #1596, #4058 ) ;
#12566 = VERTEX_POINT ( 'NONE', #790 ) ;
#12567 = EDGE_LOOP ( 'NONE', ( #10449, #14754, #5089, #888 ) ) ;
#12568 = ORIENTED_EDGE ( 'NONE', *, *, #11492, .F. ) ;
#12569 = PRODUCT_DEFINITION_CONTEXT ( 'detailed design', #12307, 'design' ) ;
#12570 = AXIS2_PLACEMENT_3D ( 'NONE', #9334, #2444, #3590 ) ;
#12571 = FACE_OUTER_BOUND ( 'NONE', #7637, .T. ) ;
#12572 = ORIENTED_EDGE ( 'NONE', *, *, #12128, .F. ) ;
#12573 = DIRECTION ( 'NONE',  ( 0.000000000000000000, 0.000000000000000000, -1.000000000000000000 ) ) ;
#12574 = CARTESIAN_POINT ( 'NONE',  ( 3.873439288382781065, 3.567999999999999616, 6.065921084684207584E-32 ) ) ;
#12575 = DIRECTION ( 'NONE',  ( -1.000000000000000000, 0.000000000000000000, 0.000000000000000000 ) ) ;
#12576 = DIRECTION ( 'NONE',  ( 0.000000000000000000, 1.000000000000000000, 0.000000000000000000 ) ) ;
#12577 = VERTEX_POINT ( 'NONE', #4192 ) ;
#12578 = B_SPLINE_CURVE_WITH_KNOTS ( 'NONE', 3,
 ( #26, #7107, #11753, #14031, #15114, #1406, #10682, #2424, #97, #3417, #3490, #6019, #4718, #1254 ),
 .UNSPECIFIED., .F., .F.,
 ( 4, 2, 2, 2, 2, 2, 4 ),
 ( 0.000000000000000000, 0.0007185039784458951626, 0.001437007956891790325, 0.001796259946114739424, 0.002155511935337688957, 0.002514763924560637839, 0.002874015913783587155 ),
 .UNSPECIFIED. ) ;
#12579 = DIRECTION ( 'NONE',  ( 1.000000000000000000, 0.000000000000000000, 0.000000000000000000 ) ) ;
#12580 = CARTESIAN_POINT ( 'NONE',  ( 0.7010945348274493227, 0.003367250660063846480, -0.4266201320538819397 ) ) ;
#12581 = DIRECTION ( 'NONE',  ( -0.9999002670844991947, 0.000000000000000000, -0.01412288512831585095 ) ) ;
#12582 = EDGE_CURVE ( 'NONE', #10975, #7670, #11145, .T. ) ;
#12583 = CONICAL_SURFACE ( 'NONE', #6014, 0.6412116890856960350, 1.326062729686469988 ) ;
#12584 = ADVANCED_FACE ( 'NONE', ( #13577 ), #2887, .T. ) ;
#12585 = CIRCLE ( 'NONE', #1595, 0.2944999999999856066 ) ;
#12586 = CIRCLE ( 'NONE', #4551, 0.05999999999999990757 ) ;
#12587 = CARTESIAN_POINT ( 'NONE',  ( -0.4349147617188193760, 1.559103846021574480, -0.008611041693309614414 ) ) ;
#12588 = CARTESIAN_POINT ( 'NONE',  ( 4.640170961443040198, 1.726011380923590188, 0.2628431377593381524 ) ) ;
#12590 = ORIENTED_EDGE ( 'NONE', *, *, #13859, .T. ) ;
#12589 = CARTESIAN_POINT ( 'NONE',  ( 0.3725000000000000533, 0.1749999999999999889, 0.3724999999999999978 ) ) ;
#12591 = EDGE_CURVE ( 'NONE', #6934, #11668, #562, .T. ) ;
#12592 = ORIENTED_EDGE ( 'NONE', *, *, #13054, .F. ) ;
#12594 = EDGE_LOOP ( 'NONE', ( #15085, #11940, #9254, #453 ) ) ;
#12593 = CYLINDRICAL_SURFACE ( 'NONE', #7255, 2.500000000000000000 ) ;
#12595 = EDGE_LOOP ( 'NONE', ( #8106, #1238, #9157, #5176 ) ) ;
#12596 = EDGE_CURVE ( 'NONE', #2681, #4332, #12189, .T. ) ;
#12597 = CARTESIAN_POINT ( 'NONE',  ( 2.774999999999999911, -1.575000000000027489, -2.359999999999986109 ) ) ;
#12598 = CARTESIAN_POINT ( 'NONE',  ( 0.000000000000000000, 0.000000000000000000, 0.000000000000000000 ) ) ;
#12599 = DIRECTION ( 'NONE',  ( -1.000000000000000000, 0.000000000000000000, 0.000000000000000000 ) ) ;
#12600 = ORIENTED_EDGE ( 'NONE', *, *, #3850, .F. ) ;
#12601 = CARTESIAN_POINT ( 'NONE',  ( 2.124999999999999556, -1.575000000000000178, 2.360000000000016751 ) ) ;
#12602 = CARTESIAN_POINT ( 'NONE',  ( 0.6500000000000001332, 1.679378605318059492, 1.679378605318041506 ) ) ;
#12603 = DIRECTION ( 'NONE',  ( -1.000000000000000000, -0.000000000000000000, -0.000000000000000000 ) ) ;
#12604 = CARTESIAN_POINT ( 'NONE',  ( 6.794491571325179891, -1.679378605318048390, 1.304378605318053497 ) ) ;
#12605 = CARTESIAN_POINT ( 'NONE',  ( 2.279764930209268847, 0.5637746725395378355, -0.4072339235673128610 ) ) ;
#12606 = DIRECTION ( 'NONE',  ( 0.000000000000000000, 0.000000000000000000, -1.000000000000000000 ) ) ;
#12607 = CARTESIAN_POINT ( 'NONE',  ( 2.650000000000001688, 0.000000000000000000, -1.000000000000000000 ) ) ;
#12608 = CIRCLE ( 'NONE', #3830, 0.2624999999999852451 ) ;
#12609 = DIRECTION ( 'NONE',  ( 0.8682164115033652596, 0.000000000000000000, -0.4961857140186719528 ) ) ;
#12610 =( BOUNDED_CURVE ( )  B_SPLINE_CURVE ( 3, ( #9106, #7958, #2213, #4593 ),
 .UNSPECIFIED., .F., .F. ) 
 B_SPLINE_CURVE_WITH_KNOTS ( ( 4, 4 ),
 ( 3.926990816987239619, 4.712388980384689674 ),
 .UNSPECIFIED. ) 
 CURVE ( )  GEOMETRIC_REPRESENTATION_ITEM ( )  RATIONAL_B_SPLINE_CURVE ( ( 1.000000000000000000, 0.9492530216741910110, 0.9492530216741910110, 1.000000000000000000 ) ) 
 REPRESENTATION_ITEM ( '' )  );
#12611 = CARTESIAN_POINT ( 'NONE',  ( 3.743903362372427601, 0.8757526003188027541, -0.4827919802056128140 ) ) ;
#12612 = DIRECTION ( 'NONE',  ( -0.000000000000000000, -1.000000000000000000, -0.000000000000000000 ) ) ;
#12613 = EDGE_CURVE ( 'NONE', #14557, #11117, #2131, .T. ) ;
#12614 = CYLINDRICAL_SURFACE ( 'NONE', #10649, 0.2624999999999852451 ) ;
#12615 = AXIS2_PLACEMENT_3D ( 'NONE', #12135, #12060, #10992 ) ;
#12617 = ORIENTED_EDGE ( 'NONE', *, *, #5685, .T. ) ;
#12616 = LINE ( 'NONE', #6668, #14558 ) ;
#12618 = ORIENTED_EDGE ( 'NONE', *, *, #13935, .T. ) ;
#12619 = EDGE_CURVE ( 'NONE', #1160, #1793, #14381, .T. ) ;
#12620 = DIRECTION ( 'NONE',  ( -0.000000000000000000, 1.000000000000000000, -0.000000000000000000 ) ) ;
#12621 = ORIENTED_EDGE ( 'NONE', *, *, #14722, .F. ) ;
#12622 = CARTESIAN_POINT ( 'NONE',  ( 2.774999999999999911, -2.360000000000016751, -0.9799999999999431388 ) ) ;
#12623 = EDGE_CURVE ( 'NONE', #9538, #3778, #690, .T. ) ;
#12624 = VECTOR ( 'NONE', #5480, 39.37007874015748854 ) ;
#12625 = CARTESIAN_POINT ( 'NONE',  ( 3.874999999999999556, 2.750000000000000000, -1.542000000000000037 ) ) ;
#12626 = CARTESIAN_POINT ( 'NONE',  ( 2.124999999999999556, -1.679378605318059048, -1.679378605318041950 ) ) ;
#12627 = DIRECTION ( 'NONE',  ( 0.000000000000000000, 0.000000000000000000, -1.000000000000000000 ) ) ;
#12628 = CARTESIAN_POINT ( 'NONE',  ( -0.4108223460329263887, 4.529999999999999361, -0.2850000000000038058 ) ) ;
#12629 = VECTOR ( 'NONE', #14281, 39.37007874015748854 ) ;
#12630 = ORIENTED_EDGE ( 'NONE', *, *, #12757, .T. ) ;
#12631 = DIRECTION ( 'NONE',  ( -0.7071067811865452413, 8.659560562354959975E-17, -0.7071067811865496822 ) ) ;
#12632 = CARTESIAN_POINT ( 'NONE',  ( 3.874999999999999556, 3.137999999999999901, -1.320000000000000062 ) ) ;
#12633 = ORIENTED_EDGE ( 'NONE', *, *, #12985, .T. ) ;
#12634 = DIRECTION ( 'NONE',  ( -0.03489949670249406499, 0.9993908270190959842, 0.000000000000000000 ) ) ;
#12635 = VERTEX_POINT ( 'NONE', #641 ) ;
#12636 = CIRCLE ( 'NONE', #5608, 0.06000000000000002554 ) ;
#12637 = CARTESIAN_POINT ( 'NONE',  ( 1.863568193433660758, 0.06187774891384333065, 0.4736784153469821290 ) ) ;
#12638 = ORIENTED_EDGE ( 'NONE', *, *, #156, .F. ) ;
#12639 = DIRECTION ( 'NONE',  ( -0.000000000000000000, -1.000000000000000000, -0.000000000000000000 ) ) ;
#12640 = AXIS2_PLACEMENT_3D ( 'NONE', #12850, #3760, #11938 ) ;
#12641 = CARTESIAN_POINT ( 'NONE',  ( 0.4850000000000000977, 1.109999999999999876, 0.000000000000000000 ) ) ;
#12642 = EDGE_CURVE ( 'NONE', #638, #3395, #4110, .T. ) ;
#12643 = LINE ( 'NONE', #4325, #7344 ) ;
#12644 = CARTESIAN_POINT ( 'NONE',  ( 3.693889022407033096, 1.943894859932088881, 0.4666066016349538215 ) ) ;
#12645 = VECTOR ( 'NONE', #3862, 39.37007874015748143 ) ;
#12646 = CARTESIAN_POINT ( 'NONE',  ( 8.707077114626732950, 0.8770090228648390607, 0.3011897810131113906 ) ) ;
#12647 = CIRCLE ( 'NONE', #12911, 0.1150000000000000050 ) ;
#12648 = CARTESIAN_POINT ( 'NONE',  ( 3.964297589650334075, 1.829743176842955510, -0.7450599964799213826 ) ) ;
#12649 = VERTEX_POINT ( 'NONE', #720 ) ;
#12650 = VECTOR ( 'NONE', #14470, 39.37007874015748854 ) ;
#12651 = VERTEX_POINT ( 'NONE', #14583 ) ;
#12652 = AXIS2_PLACEMENT_3D ( 'NONE', #7132, #55, #13908 ) ;
#12653 = DIRECTION ( 'NONE',  ( 0.7070715176384831935, 0.7070715176384805289, -0.009986885842351451645 ) ) ;
#12654 = ORIENTED_EDGE ( 'NONE', *, *, #10795, .F. ) ;
#12655 = TOROIDAL_SURFACE ( 'NONE', #9974, 1.409999999999999920, 0.05999999999999999778 ) ;
#12656 = CARTESIAN_POINT ( 'NONE',  ( 0.4193214606628480889, 1.577645543303439313, -0.03561943137997464898 ) ) ;
#12657 = FACE_OUTER_BOUND ( 'NONE', #2198, .T. ) ;
#12659 = CARTESIAN_POINT ( 'NONE',  ( 0.3190000000000000058, 1.159999999999999698, 0.000000000000000000 ) ) ;
#12658 = AXIS2_PLACEMENT_3D ( 'NONE', #438, #14076, #3614 ) ;
#12660 = DIRECTION ( 'NONE',  ( -0.4961857140186717308, -0.000000000000000000, 0.8682164115033652596 ) ) ;
#12661 = ORIENTED_EDGE ( 'NONE', *, *, #13918, .T. ) ;
#12662 = EDGE_CURVE ( 'NONE', #14785, #7387, #6343, .T. ) ;
#12663 = DIRECTION ( 'NONE',  ( 0.000000000000000000, 1.000000000000000000, 0.000000000000000000 ) ) ;
#12664 = CARTESIAN_POINT ( 'NONE',  ( 0.7204397385173409996, -0.006614428813630259842, -0.4582225808237102571 ) ) ;
#12665 = DIRECTION ( 'NONE',  ( 8.659560562355030233E-17, 0.7071067811865392461, -0.7071067811865555663 ) ) ;
#12666 = VECTOR ( 'NONE', #5209, 39.37007874015748143 ) ;
#12667 = CIRCLE ( 'NONE', #6092, 0.7406097974541305806 ) ;
#12668 =( GEOMETRIC_REPRESENTATION_CONTEXT ( 3 ) GLOBAL_UNCERTAINTY_ASSIGNED_CONTEXT ( ( #12728 ) ) GLOBAL_UNIT_ASSIGNED_CONTEXT ( ( #8731, #13162, #4151 ) ) REPRESENTATION_CONTEXT ( 'NONE', 'WORKASPACE' ) );
#12669 = DIRECTION ( 'NONE',  ( -0.000000000000000000, -1.000000000000000000, -0.000000000000000000 ) ) ;
#12670 = AXIS2_PLACEMENT_3D ( 'NONE', #5945, #8471, #3729 ) ;
#12671 = CARTESIAN_POINT ( 'NONE',  ( 4.625991625415837305, 1.810439985556918430, -0.03431761865087439717 ) ) ;
#12673 = ORIENTED_EDGE ( 'NONE', *, *, #1938, .T. ) ;
#12672 = DIRECTION ( 'NONE',  ( 1.000000000000000000, 0.000000000000000000, 0.000000000000000000 ) ) ;
#12674 = EDGE_LOOP ( 'NONE', ( #1951, #11054, #11075, #12395 ) ) ;
#12676 = ORIENTED_EDGE ( 'NONE', *, *, #8963, .T. ) ;
#12675 = DIRECTION ( 'NONE',  ( 0.000000000000000000, 0.000000000000000000, 1.000000000000000000 ) ) ;
#12677 = ORIENTED_EDGE ( 'NONE', *, *, #12724, .T. ) ;
#12678 = EDGE_CURVE ( 'NONE', #6416, #4777, #935, .T. ) ;
#12679 = EDGE_CURVE ( 'NONE', #9898, #3117, #10698, .T. ) ;
#12680 = DIRECTION ( 'NONE',  ( -0.9999002670844991947, 0.000000000000000000, -0.01412288512831213171 ) ) ;
#12681 = DIRECTION ( 'NONE',  ( -4.857225732735059248E-17, -0.9510348695591864798, 0.3090836082398114026 ) ) ;
#12682 = CARTESIAN_POINT ( 'NONE',  ( -0.3725000000000000533, -0.6590000000000000302, 0.3724999999999999423 ) ) ;
#12683 = ORIENTED_EDGE ( 'NONE', *, *, #6344, .F. ) ;
#12684 = EDGE_CURVE ( 'NONE', #1691, #2057, #7625, .T. ) ;
#12685 =( GEOMETRIC_REPRESENTATION_CONTEXT ( 3 ) GLOBAL_UNCERTAINTY_ASSIGNED_CONTEXT ( ( #4333 ) ) GLOBAL_UNIT_ASSIGNED_CONTEXT ( ( #14625, #4158, #3079 ) ) REPRESENTATION_CONTEXT ( 'NONE', 'WORKASPACE' ) );
#12686 = DIRECTION ( 'NONE',  ( -1.000000000000000000, -0.000000000000000000, -0.000000000000000000 ) ) ;
#12687 = CARTESIAN_POINT ( 'NONE',  ( 4.212784989066894333E-17, 1.503199999999999870, 0.3439999999999999170 ) ) ;
#12688 = CONICAL_SURFACE ( 'NONE', #6109, 1.000000000000000000, 0.7853981633974517207 ) ;
#12689 = DIRECTION ( 'NONE',  ( 0.9999002670844989726, 0.000000000000000000, -0.01412288512831212997 ) ) ;
#12690 = CARTESIAN_POINT ( 'NONE',  ( 3.875000000000000000, 3.567999999999999616, 0.000000000000000000 ) ) ;
#12691 = EDGE_CURVE ( 'NONE', #12259, #14862, #3159, .T. ) ;
#12692 = FACE_OUTER_BOUND ( 'NONE', #2040, .T. ) ;
#12693 = DIRECTION ( 'NONE',  ( 1.000000000000000000, 0.000000000000000000, 0.000000000000000000 ) ) ;
#12694 = LINE ( 'NONE', #1054, #5842 ) ;
#12695 = CARTESIAN_POINT ( 'NONE',  ( 3.712368062279605141, 0.8810275311047641722, 0.4730969127157453880 ) ) ;
#12696 = CARTESIAN_POINT ( 'NONE',  ( 2.774999999999999911, -1.574999999999999956, 2.360000000000024745 ) ) ;
#12697 = AXIS2_PLACEMENT_3D ( 'NONE', #11708, #10121, #14774 ) ;
#12698 = DIRECTION ( 'NONE',  ( 0.000000000000000000, 0.000000000000000000, -1.000000000000000000 ) ) ;
#12700 = ORIENTED_EDGE ( 'NONE', *, *, #7538, .F. ) ;
#12699 = FACE_OUTER_BOUND ( 'NONE', #1233, .T. ) ;
#12701 = ORIENTED_EDGE ( 'NONE', *, *, #4214, .F. ) ;
#12702 = CARTESIAN_POINT ( 'NONE',  ( 0.000000000000000000, -1.002374524060224757E-18, 0.000000000000000000 ) ) ;
#12703 = ORIENTED_EDGE ( 'NONE', *, *, #4311, .T. ) ;
#12704 = DIRECTION ( 'NONE',  ( 1.000000000000000000, 0.000000000000000000, 0.000000000000000000 ) ) ;
#12705 = CARTESIAN_POINT ( 'NONE',  ( 2.854443715606263865, 0.5365358177141184015, -0.4001101571913185384 ) ) ;
#12706 = DIRECTION ( 'NONE',  ( 0.000000000000000000, 0.000000000000000000, -1.000000000000000000 ) ) ;
#12707 = CARTESIAN_POINT ( 'NONE',  ( 3.874999999999999556, 2.782000000000002693, 1.320000000000000062 ) ) ;
#12708 = EDGE_CURVE ( 'NONE', #7657, #12462, #11712, .T. ) ;
#12709 = ORIENTED_EDGE ( 'NONE', *, *, #12691, .T. ) ;
#12710 = CARTESIAN_POINT ( 'NONE',  ( 0.7134904538003045138, -0.4430000000000007265, 0.4077598229816897235 ) ) ;
#12711 = CARTESIAN_POINT ( 'NONE',  ( 3.875000000000000000, 1.112678268764263789, 0.5849999999999996314 ) ) ;
#12712 = ORIENTED_EDGE ( 'NONE', *, *, #14840, .F. ) ;
#12713 = EDGE_CURVE ( 'NONE', #3646, #5710, #14144, .T. ) ;
#12714 = CIRCLE ( 'NONE', #2212, 0.2624999999999852451 ) ;
#12715 = CARTESIAN_POINT ( 'NONE',  ( 8.849999999999999645, 0.9969999999999998863, 6.829619984160658046E-17 ) ) ;
#12716 = DIRECTION ( 'NONE',  ( -0.7071067811865447972, 8.659560562354964906E-17, -0.7071067811865501263 ) ) ;
#12717 = CARTESIAN_POINT ( 'NONE',  ( 0.000000000000000000, 1.000000000000000000, 0.6614378277661475680 ) ) ;
#12718 = EDGE_LOOP ( 'NONE', ( #7210, #12195, #6176, #9037 ) ) ;
#12719 = DIRECTION ( 'NONE',  ( 0.000000000000000000, 0.000000000000000000, -1.000000000000000000 ) ) ;
#12720 = DIRECTION ( 'NONE',  ( 0.000000000000000000, 0.000000000000000000, -1.000000000000000000 ) ) ;
#12721 = LINE ( 'NONE', #4552, #8512 ) ;
#12722 = CIRCLE ( 'NONE', #5407, 0.2625000000000000111 ) ;
#12723 = DIRECTION ( 'NONE',  ( -0.000000000000000000, -1.000000000000000000, -0.000000000000000000 ) ) ;
#12724 = EDGE_CURVE ( 'NONE', #7890, #6474, #1187, .T. ) ;
#12725 = EDGE_CURVE ( 'NONE', #8139, #11449, #1677, .T. ) ;
#12726 = ORIENTED_EDGE ( 'NONE', *, *, #2773, .F. ) ;
#12727 = ORIENTED_EDGE ( 'NONE', *, *, #1279, .T. ) ;
#12728 = UNCERTAINTY_MEASURE_WITH_UNIT (LENGTH_MEASURE( 1.000000000000000082E-05 ), #8731, 'distance_accuracy_value', 'NONE');
#12729 = CARTESIAN_POINT ( 'NONE',  ( 1.010189475225347078, -0.4429749903950104262, -0.4085521775708274572 ) ) ;
#12730 = ORIENTED_EDGE ( 'NONE', *, *, #3723, .T. ) ;
#12731 = CIRCLE ( 'NONE', #2492, 3.000000000000000444 ) ;
#12732 = CARTESIAN_POINT ( 'NONE',  ( 2.807059454666800402, 0.6196377705552925663, -0.4603522675894519689 ) ) ;
#12733 = CARTESIAN_POINT ( 'NONE',  ( 0.9022048395661492748, -0.4607945367651646862, -0.4500484056301596314 ) ) ;
#12734 = DIRECTION ( 'NONE',  ( -0.000000000000000000, -1.000000000000000000, 0.000000000000000000 ) ) ;
#12735 = CARTESIAN_POINT ( 'NONE',  ( -0.3725000000000002198, -0.6590000000000000302, -0.3725000000000000533 ) ) ;
#12736 = ORIENTED_EDGE ( 'NONE', *, *, #1157, .T. ) ;
#12737 = CARTESIAN_POINT ( 'NONE',  ( 3.874999999999999556, 3.567999999999999616, 1.320000000000000062 ) ) ;
#12738 = CARTESIAN_POINT ( 'NONE',  ( 0.7040204553985035529, -0.05593285129442519821, -0.4900562082570833478 ) ) ;
#12739 = CARTESIAN_POINT ( 'NONE',  ( 2.774999999999999911, 1.575000000000016387, 2.359999999999999876 ) ) ;
#12740 = ADVANCED_FACE ( 'NONE', ( #11370 ), #5703, .F. ) ;
#12741 = CARTESIAN_POINT ( 'NONE',  ( 4.612938997950140951, 1.807748895277201839, 0.1434262448729105577 ) ) ;
#12743 = ORIENTED_EDGE ( 'NONE', *, *, #3634, .F. ) ;
#12742 = CARTESIAN_POINT ( 'NONE',  ( 0.4349147617188415249, 1.559103846021539619, 0.008611041693268213504 ) ) ;
#12744 = VERTEX_POINT ( 'NONE', #7857 ) ;
#12746 = VERTEX_POINT ( 'NONE', #1030 ) ;
#12745 = CARTESIAN_POINT ( 'NONE',  ( 3.875000000000000000, 3.567999999999999616, -0.4849999999999995981 ) ) ;
#12747 = ORIENTED_EDGE ( 'NONE', *, *, #14233, .T. ) ;
#12748 = VECTOR ( 'NONE', #3924, 39.37007874015748143 ) ;
#12749 = CARTESIAN_POINT ( 'NONE',  ( -0.3724999999999999423, 0.000000000000000000, 0.4124999999999999778 ) ) ;
#12750 = DIRECTION ( 'NONE',  ( -0.000000000000000000, -1.000000000000000000, -0.000000000000000000 ) ) ;
#12751 = ORIENTED_EDGE ( 'NONE', *, *, #11686, .F. ) ;
#12752 = DIRECTION ( 'NONE',  ( -1.000000000000000000, -0.000000000000000000, -0.000000000000000000 ) ) ;
#12753 = CARTESIAN_POINT ( 'NONE',  ( 0.6601485485260571995, -0.3723516483516483011, -0.5137583810202324131 ) ) ;
#12754 = CARTESIAN_POINT ( 'NONE',  ( 3.874999999999999556, 2.782000000000002693, 1.320000000000000062 ) ) ;
#12755 = DIRECTION ( 'NONE',  ( 0.000000000000000000, 0.000000000000000000, -1.000000000000000000 ) ) ;
#12756 = AXIS2_PLACEMENT_3D ( 'NONE', #2819, #7414, #5051 ) ;
#12757 = EDGE_CURVE ( 'NONE', #4756, #9216, #12636, .T. ) ;
#12758 = DIRECTION ( 'NONE',  ( 0.000000000000000000, 0.000000000000000000, -1.000000000000000000 ) ) ;
#12759 = AXIS2_PLACEMENT_3D ( 'NONE', #1284, #8359, #5825 ) ;
#12760 = FACE_OUTER_BOUND ( 'NONE', #13486, .T. ) ;
#12761 = EDGE_CURVE ( 'NONE', #1733, #5075, #6721, .T. ) ;
#12762 = CARTESIAN_POINT ( 'NONE',  ( 3.426491571325181340, 0.9800000000000039790, 3.360000000000000320 ) ) ;
#12763 = CARTESIAN_POINT ( 'NONE',  ( 2.061999999999999389, 1.812000000000000277, 0.000000000000000000 ) ) ;
#12764 = CARTESIAN_POINT ( 'NONE',  ( 4.586868767028525973, 1.718843021825377626, 0.3797541001213830536 ) ) ;
#12765 = VERTEX_POINT ( 'NONE', #6710 ) ;
#12766 = FACE_OUTER_BOUND ( 'NONE', #8898, .T. ) ;
#12768 = EDGE_LOOP ( 'NONE', ( #1098, #12155, #4163, #63 ) ) ;
#12767 = DIRECTION ( 'NONE',  ( 0.000000000000000000, 0.000000000000000000, 1.000000000000000000 ) ) ;
#12769 = ORIENTED_EDGE ( 'NONE', *, *, #3869, .T. ) ;
#12770 = EDGE_CURVE ( 'NONE', #5690, #13527, #4097, .T. ) ;
#12771 = CARTESIAN_POINT ( 'NONE',  ( 0.000000000000000000, 0.000000000000000000, 0.000000000000000000 ) ) ;
#12772 = ORIENTED_EDGE ( 'NONE', *, *, #1632, .T. ) ;
#12773 = CARTESIAN_POINT ( 'NONE',  ( 0.000000000000000000, 1.610000000000000098, 0.000000000000000000 ) ) ;
#12774 = CARTESIAN_POINT ( 'NONE',  ( 0.000000000000000000, 0.1749999999999999889, 0.000000000000000000 ) ) ;
#12775 = ADVANCED_FACE ( 'NONE', ( #10231 ), #7275, .T. ) ;
#12776 = DIRECTION ( 'NONE',  ( 1.000000000000000000, 1.874307916738609066E-16, 0.000000000000000000 ) ) ;
#12777 = AXIS2_PLACEMENT_3D ( 'NONE', #1836, #3158, #14847 ) ;
#12778 = ORIENTED_EDGE ( 'NONE', *, *, #235, .F. ) ;
#12779 = CONICAL_SURFACE ( 'NONE', #6209, 1.350000000000000089, 0.2094395102393122321 ) ;
#12780 = ADVANCED_FACE ( 'NONE', ( #1559 ), #1258, .F. ) ;
#12781 = CARTESIAN_POINT ( 'NONE',  ( 0.6570965961311159287, -0.3875664237315883387, 0.5130374278108668085 ) ) ;
#12782 = DIRECTION ( 'NONE',  ( -0.3420201433256621071, 0.000000000000000000, 0.9396926207859108704 ) ) ;
#12783 = CARTESIAN_POINT ( 'NONE',  ( 0.6179999999999962190, -1.679378605318048390, 1.679378605318054163 ) ) ;
#12784 = EDGE_LOOP ( 'NONE', ( #10696, #13681, #2998, #12592 ) ) ;
#12785 = DIRECTION ( 'NONE',  ( 0.000000000000000000, 0.000000000000000000, -1.000000000000000000 ) ) ;
#12786 = ORIENTED_EDGE ( 'NONE', *, *, #12216, .F. ) ;
#12787 = CARTESIAN_POINT ( 'NONE',  ( 0.7513246802501661881, -0.4429999999999998939, -0.4293820849162031661 ) ) ;
#12788 = DIRECTION ( 'NONE',  ( -0.000000000000000000, -1.000000000000000000, -0.000000000000000000 ) ) ;
#12789 = ORIENTED_EDGE ( 'NONE', *, *, #9360, .F. ) ;
#12790 = AXIS2_PLACEMENT_3D ( 'NONE', #1050, #7876, #10556 ) ;
#12791 = EDGE_CURVE ( 'NONE', #694, #9791, #7178, .T. ) ;
#12792 = DIRECTION ( 'NONE',  ( 0.000000000000000000, 0.000000000000000000, 1.000000000000000000 ) ) ;
#12793 = DIRECTION ( 'NONE',  ( 0.000000000000000000, 0.000000000000000000, -1.000000000000000000 ) ) ;
#12794 = EDGE_CURVE ( 'NONE', #651, #4021, #6022, .T. ) ;
#12795 = CARTESIAN_POINT ( 'NONE',  ( 2.743000000000000771, 1.679378605318059048, 1.679378605318041506 ) ) ;
#12796 = AXIS2_PLACEMENT_3D ( 'NONE', #13447, #14604, #5364 ) ;
#12797 = DIRECTION ( 'NONE',  ( 0.000000000000000000, 0.000000000000000000, 1.000000000000000000 ) ) ;
#12798 = PRODUCT_DEFINITION_FORMATION_WITH_SPECIFIED_SOURCE ( 'ANY', '', #6544, .NOT_KNOWN. ) ;
#12799 = CARTESIAN_POINT ( 'NONE',  ( 3.643830797058309479, 1.947962297878459204, -0.7137606667491679380 ) ) ;
#12800 = ORIENTED_EDGE ( 'NONE', *, *, #10170, .F. ) ;
#12801 = ORIENTED_EDGE ( 'NONE', *, *, #5487, .F. ) ;
#12802 = EDGE_CURVE ( 'NONE', #14777, #8189, #11423, .T. ) ;
#12803 = CARTESIAN_POINT ( 'NONE',  ( 1.014924625165573246, -0.4429443310102024189, -0.3808900809060754011 ) ) ;
#12804 = ORIENTED_EDGE ( 'NONE', *, *, #14541, .T. ) ;
#12805 = LINE ( 'NONE', #9388, #7752 ) ;
#12806 = CARTESIAN_POINT ( 'NONE',  ( 3.874999999999999556, 3.137999999999999901, -1.098000000000000087 ) ) ;
#12807 = CIRCLE ( 'NONE', #5494, 0.2625000000000000111 ) ;
#12808 = DIRECTION ( 'NONE',  ( 0.000000000000000000, 0.000000000000000000, -1.000000000000000000 ) ) ;
#12809 = EDGE_LOOP ( 'NONE', ( #11462, #8690, #10615, #6445 ) ) ;
#12810 = FACE_OUTER_BOUND ( 'NONE', #6747, .T. ) ;
#12811 = AXIS2_PLACEMENT_3D ( 'NONE', #10278, #8899, #5536 ) ;
#12812 = CIRCLE ( 'NONE', #101, 0.4070000000000022489 ) ;
#12813 = EDGE_CURVE ( 'NONE', #7174, #14092, #7328, .T. ) ;
#12814 = CARTESIAN_POINT ( 'NONE',  ( 3.426491571325181340, 3.360000000000000320, -0.9800000000000012035 ) ) ;
#12815 = FACE_OUTER_BOUND ( 'NONE', #10661, .T. ) ;
#12816 = DIRECTION ( 'NONE',  ( 0.000000000000000000, 0.000000000000000000, -1.000000000000000000 ) ) ;
#12817 = CYLINDRICAL_SURFACE ( 'NONE', #5944, 0.4999999999999997224 ) ;
#12818 = CARTESIAN_POINT ( 'NONE',  ( 4.593428806625106553, 1.719801573518523474, -0.3651073496023718445 ) ) ;
#12819 = ORIENTED_EDGE ( 'NONE', *, *, #8091, .T. ) ;
#12820 = VECTOR ( 'NONE', #6732, 39.37007874015748854 ) ;
#12822 = EDGE_LOOP ( 'NONE', ( #5018, #9299, #10368, #4256 ) ) ;
#12821 = CARTESIAN_POINT ( 'NONE',  ( 0.2324059764400484562, 1.569496918332968782, 0.3593665467752015230 ) ) ;
#12823 = CIRCLE ( 'NONE', #4784, 0.3750000000000004996 ) ;
#12824 = EDGE_LOOP ( 'NONE', ( #8618, #2445 ) ) ;
#12825 = ORIENTED_EDGE ( 'NONE', *, *, #12216, .T. ) ;
#12826 = VERTEX_POINT ( 'NONE', #14260 ) ;
#12827 = LINE ( 'NONE', #1122, #1863 ) ;
#12828 = DIRECTION ( 'NONE',  ( 0.000000000000000000, 0.000000000000000000, 1.000000000000000000 ) ) ;
#12829 = FACE_OUTER_BOUND ( 'NONE', #9862, .T. ) ;
#12830 = ORIENTED_EDGE ( 'NONE', *, *, #5708, .F. ) ;
#12831 = FACE_OUTER_BOUND ( 'NONE', #5270, .T. ) ;
#12832 = FACE_OUTER_BOUND ( 'NONE', #12858, .T. ) ;
#12833 = EDGE_CURVE ( 'NONE', #3096, #13193, #11905, .T. ) ;
#12834 = AXIS2_PLACEMENT_3D ( 'NONE', #7303, #10808, #3853 ) ;
#12835 = CARTESIAN_POINT ( 'NONE',  ( 3.874999999999999556, 3.535499999999999421, -1.320000000000000062 ) ) ;
#12836 = CARTESIAN_POINT ( 'NONE',  ( -0.4349147617188414139, 1.559103846021539619, 0.008611041693274201769 ) ) ;
#12837 = VECTOR ( 'NONE', #3330, 39.37007874015748143 ) ;
#12838 = CARTESIAN_POINT ( 'NONE',  ( 6.826491571325181695, -1.679378605318048390, 2.086378605318056412 ) ) ;
#12839 = CARTESIAN_POINT ( 'NONE',  ( 3.426491571325181340, -1.679378605318059048, -1.384878605318056399 ) ) ;
#12840 = CARTESIAN_POINT ( 'NONE',  ( 0.8999999999999999112, -0.6429999999999999050, -0.3199999999999985634 ) ) ;
#12841 = CARTESIAN_POINT ( 'NONE',  ( 0.8999999999999999112, -0.6429999999999999050, -0.3750000000000000555 ) ) ;
#12842 = CARTESIAN_POINT ( 'NONE',  ( 4.646274775377375654, 1.726933778515093332, 0.2437811747078761637 ) ) ;
#12843 = VERTEX_POINT ( 'NONE', #10766 ) ;
#12844 = DIRECTION ( 'NONE',  ( 0.000000000000000000, 0.000000000000000000, -1.000000000000000000 ) ) ;
#12846 = ORIENTED_EDGE ( 'NONE', *, *, #13370, .F. ) ;
#12845 = PLANE ( 'NONE',  #13083 ) ;
#12847 = ORIENTED_EDGE ( 'NONE', *, *, #12802, .T. ) ;
#12848 = AXIS2_PLACEMENT_3D ( 'NONE', #8632, #7413, #13276 ) ;
#12849 = AXIS2_PLACEMENT_3D ( 'NONE', #5465, #1934, #14716 ) ;
#12850 = CARTESIAN_POINT ( 'NONE',  ( 3.873439288382781065, 3.567999999999999616, 6.065921084684207584E-32 ) ) ;
#12851 = CARTESIAN_POINT ( 'NONE',  ( 3.944129661530210385, 0.000000000000000000, 0.000000000000000000 ) ) ;
#12852 = ORIENTED_EDGE ( 'NONE', *, *, #2184, .F. ) ;
#12853 = FACE_OUTER_BOUND ( 'NONE', #4225, .T. ) ;
#12854 = PRODUCT_RELATED_PRODUCT_CATEGORY ( 'part', '', ( #5185 ) ) ;
#12855 = VECTOR ( 'NONE', #11538, 39.37007874015748143 ) ;
#12856 = CARTESIAN_POINT ( 'NONE',  ( 2.743000000000000327, 1.679378605318042395, -1.679378605318058604 ) ) ;
#12857 = PLANE ( 'NONE',  #2167 ) ;
#12858 = EDGE_LOOP ( 'NONE', ( #10937, #7016, #10663, #5934 ) ) ;
#12859 = CARTESIAN_POINT ( 'NONE',  ( 0.6757966763796152687, -0.3817220302227288253, 0.4909001136279363409 ) ) ;
#12860 = CIRCLE ( 'NONE', #12615, 0.2944999999999976525 ) ;
#12861 = CARTESIAN_POINT ( 'NONE',  ( 4.344846310392954436, 3.137999999999999901, -1.491010071662831171 ) ) ;
#12862 = CARTESIAN_POINT ( 'NONE',  ( 3.874999999999999556, 2.750000000000000000, -1.098000000000000087 ) ) ;
#12863 = ORIENTED_EDGE ( 'NONE', *, *, #6175, .T. ) ;
#12864 = DIRECTION ( 'NONE',  ( -0.000000000000000000, 1.000000000000000000, -0.000000000000000000 ) ) ;
#12865 = ORIENTED_EDGE ( 'NONE', *, *, #11021, .F. ) ;
#12866 = VECTOR ( 'NONE', #2734, 39.37007874015748143 ) ;
#12867 = CARTESIAN_POINT ( 'NONE',  ( 0.3724999999999997757, -0.6589999999999996971, -0.3725000000000000533 ) ) ;
#12868 = ORIENTED_EDGE ( 'NONE', *, *, #14090, .T. ) ;
#12869 = EDGE_CURVE ( 'NONE', #5558, #391, #6060, .T. ) ;
#12870 = FACE_OUTER_BOUND ( 'NONE', #10883, .T. ) ;
#12871 = EDGE_CURVE ( 'NONE', #10938, #4169, #4140, .T. ) ;
#12872 = EDGE_CURVE ( 'NONE', #10755, #10245, #13886, .T. ) ;
#12873 = AXIS2_PLACEMENT_3D ( 'NONE', #3190, #12500, #14659 ) ;
#12874 = DIRECTION ( 'NONE',  ( -2.602462600580851747E-17, -1.000000000000000000, 0.000000000000000000 ) ) ;
#12875 = DIRECTION ( 'NONE',  ( 0.000000000000000000, 0.000000000000000000, 1.000000000000000000 ) ) ;
#12876 = EDGE_CURVE ( 'NONE', #4182, #2748, #6171, .T. ) ;
#12877 = DIRECTION ( 'NONE',  ( 0.000000000000000000, 0.000000000000000000, -1.000000000000000000 ) ) ;
#12878 = ORIENTED_EDGE ( 'NONE', *, *, #10305, .F. ) ;
#12879 = AXIS2_PLACEMENT_3D ( 'NONE', #2739, #7480, #10926 ) ;
#12880 = VERTEX_POINT ( 'NONE', #9910 ) ;
#12881 = UNCERTAINTY_MEASURE_WITH_UNIT (LENGTH_MEASURE( 1.000000000000000082E-05 ), #2774, 'distance_accuracy_value', 'NONE');
#12882 = PLANE ( 'NONE',  #4302 ) ;
#12883 = ORIENTED_EDGE ( 'NONE', *, *, #3575, .F. ) ;
#12884 = FACE_OUTER_BOUND ( 'NONE', #5287, .T. ) ;
#12885 = DIRECTION ( 'NONE',  ( -0.000000000000000000, 4.591341165821855765E-15, 1.000000000000000000 ) ) ;
#12886 = PRESENTATION_STYLE_ASSIGNMENT (( #8599 ) ) ;
#12887 = DIRECTION ( 'NONE',  ( -0.9999002670844991947, 0.000000000000000000, 0.01412288512831128169 ) ) ;
#12888 = EDGE_LOOP ( 'NONE', ( #12479, #8983, #14725, #10701 ) ) ;
#12889 = DIRECTION ( 'NONE',  ( -0.000000000000000000, 1.000000000000000000, -0.000000000000000000 ) ) ;
#12890 = AXIS2_PLACEMENT_3D ( 'NONE', #3556, #9377, #7010 ) ;
#12891 = CARTESIAN_POINT ( 'NONE',  ( 1.973685276483480910, 0.1827974636779289841, 0.4721230893152050245 ) ) ;
#12892 = CARTESIAN_POINT ( 'NONE',  ( 2.837768005214870382, 0.5663408804686759224, -0.4003582515643820949 ) ) ;
#12893 = VECTOR ( 'NONE', #7780, 39.37007874015748143 ) ;
#12894 = AXIS2_PLACEMENT_3D ( 'NONE', #6899, #8046, #1133 ) ;
#12895 = EDGE_CURVE ( 'NONE', #5634, #2016, #2172, .T. ) ;
#12896 = CARTESIAN_POINT ( 'NONE',  ( 0.4124999999999999223, 0.2159999999999999698, 0.3724999999999999423 ) ) ;
#12897 = AXIS2_PLACEMENT_3D ( 'NONE', #6406, #2957, #10008 ) ;
#12898 = CARTESIAN_POINT ( 'NONE',  ( 4.626594302918601187, 1.810567462571540664, -0.01639964552859272603 ) ) ;
#12899 = ORIENTED_EDGE ( 'NONE', *, *, #11842, .F. ) ;
#12901 = EDGE_LOOP ( 'NONE', ( #10353, #10154, #11009, #2565 ) ) ;
#12900 = DIRECTION ( 'NONE',  ( 0.000000000000000000, 0.000000000000000000, 1.000000000000000000 ) ) ;
#12902 = AXIS2_PLACEMENT_3D ( 'NONE', #9654, #14379, #3695 ) ;
#12903 = EDGE_CURVE ( 'NONE', #13224, #2178, #5851, .T. ) ;
#12904 = ORIENTED_EDGE ( 'NONE', *, *, #1372, .F. ) ;
#12905 = DIRECTION ( 'NONE',  ( -1.150251786806006500E-15, 0.000000000000000000, 1.000000000000000000 ) ) ;
#12906 = ORIENTED_EDGE ( 'NONE', *, *, #9833, .T. ) ;
#12907 = DIRECTION ( 'NONE',  ( 0.4999999999999998890, 0.000000000000000000, -0.8660254037844385966 ) ) ;
#12908 = CARTESIAN_POINT ( 'NONE',  ( 3.234999999999999432, 1.679378605318042395, -1.679378605318059270 ) ) ;
#12909 = DIRECTION ( 'NONE',  ( -1.000000000000000000, 0.000000000000000000, 0.000000000000000000 ) ) ;
#12910 = ORIENTED_EDGE ( 'NONE', *, *, #4592, .T. ) ;
#12911 = AXIS2_PLACEMENT_3D ( 'NONE', #10573, #9289, #4533 ) ;
#12912 = FACE_OUTER_BOUND ( 'NONE', #4922, .T. ) ;
#12913 = CARTESIAN_POINT ( 'NONE',  ( 2.774999999999999911, 2.360000000000000320, -0.9800000000000007594 ) ) ;
#12914 = AXIS2_PLACEMENT_3D ( 'NONE', #13830, #1056, #13910 ) ;
#12915 = AXIS2_PLACEMENT_3D ( 'NONE', #5968, #15068, #126 ) ;
#12916 = FACE_OUTER_BOUND ( 'NONE', #170, .T. ) ;
#12917 = CIRCLE ( 'NONE', #933, 0.3750000000000004996 ) ;
#12918 = DIRECTION ( 'NONE',  ( -1.000000000000000000, -0.000000000000000000, -0.000000000000000000 ) ) ;
#12919 = CIRCLE ( 'NONE', #14394, 0.2225000000000001421 ) ;
#12920 = VECTOR ( 'NONE', #10081, 39.37007874015748143 ) ;
#12921 = DIRECTION ( 'NONE',  ( 0.000000000000000000, 0.000000000000000000, -1.000000000000000000 ) ) ;
#12922 = CARTESIAN_POINT ( 'NONE',  ( 2.230477600021715912, 0.4287871555018993308, -0.4684960790957384824 ) ) ;
#12923 = CARTESIAN_POINT ( 'NONE',  ( 3.667128492022511566, 0.8905039771886829048, 0.4550300979733812867 ) ) ;
#12924 = CARTESIAN_POINT ( 'NONE',  ( 4.608301153546221052, 1.721636985526682206, -0.3364488613251436222 ) ) ;
#12925 = EDGE_CURVE ( 'NONE', #11243, #14153, #3019, .T. ) ;
#12926 = VERTEX_POINT ( 'NONE', #5241 ) ;
#12927 = AXIS2_PLACEMENT_3D ( 'NONE', #6301, #2709, #4796 ) ;
#12928 = DIRECTION ( 'NONE',  ( 0.000000000000000000, 0.000000000000000000, 1.000000000000000000 ) ) ;
#12930 = ORIENTED_EDGE ( 'NONE', *, *, #11597, .F. ) ;
#12929 = CARTESIAN_POINT ( 'NONE',  ( 5.567023771132172172, 0.000000000000000000, 0.000000000000000000 ) ) ;
#12931 = EDGE_LOOP ( 'NONE', ( #11438, #1659, #12010, #13790 ) ) ;
#12932 = AXIS2_PLACEMENT_3D ( 'NONE', #5645, #12663, #6873 ) ;
#12933 = CARTESIAN_POINT ( 'NONE',  ( 0.09500000000000431710, -1.679378605318047946, -1.679378605318053497 ) ) ;
#12934 = CARTESIAN_POINT ( 'NONE',  ( 6.787121492585022509, 3.673940397442060361E-16, -3.000000000000000444 ) ) ;
#12935 = CARTESIAN_POINT ( 'NONE',  ( 3.390179639970223313, 0.6913388717410869910, 0.3921396980529558429 ) ) ;
#12936 = EDGE_LOOP ( 'NONE', ( #11022, #3108, #855, #11490 ) ) ;
#12937 = CARTESIAN_POINT ( 'NONE',  ( 3.426491571325181340, 1.575000000000016387, 2.359999999999999432 ) ) ;
#12938 = CARTESIAN_POINT ( 'NONE',  ( 3.875000000000000000, 3.085321731235734610, 0.000000000000000000 ) ) ;
#12939 = DIRECTION ( 'NONE',  ( 0.000000000000000000, 0.000000000000000000, 1.000000000000000000 ) ) ;
#12940 = VECTOR ( 'NONE', #13856, 39.37007874015748143 ) ;
#12941 = VERTEX_POINT ( 'NONE', #12269 ) ;
#12942 = CARTESIAN_POINT ( 'NONE',  ( 0.7429169091362286537, -0.4430000000000002824, 0.4367090053324595988 ) ) ;
#12943 = CYLINDRICAL_SURFACE ( 'NONE', #7398, 0.1249999999999999029 ) ;
#12944 = FACE_OUTER_BOUND ( 'NONE', #679, .T. ) ;
#12945 = ORIENTED_EDGE ( 'NONE', *, *, #2886, .F. ) ;
#12946 = CARTESIAN_POINT ( 'NONE',  ( 0.000000000000000000, 1.866025403784438819, 0.000000000000000000 ) ) ;
#12947 = LINE ( 'NONE', #154, #358 ) ;
#12948 = EDGE_CURVE ( 'NONE', #12151, #12649, #1436, .T. ) ;
#12949 = ORIENTED_EDGE ( 'NONE', *, *, #8733, .T. ) ;
#12950 = CARTESIAN_POINT ( 'NONE',  ( 1.650520655410188775, 0.1749999999999999889, -0.5816197779170857451 ) ) ;
#12951 = ORIENTED_EDGE ( 'NONE', *, *, #10218, .T. ) ;
#12952 = DIRECTION ( 'NONE',  ( 0.000000000000000000, 0.000000000000000000, -1.000000000000000000 ) ) ;
#12953 = CARTESIAN_POINT ( 'NONE',  ( 8.469665986256828205, 1.056999999999999940, 6.829619984160658046E-17 ) ) ;
#12954 = CARTESIAN_POINT ( 'NONE',  ( -0.2249147617188397563, 0.7512260236060024354, 0.3723417112827376307 ) ) ;
#12955 = EDGE_CURVE ( 'NONE', #3096, #2531, #440, .T. ) ;
#12956 = EDGE_CURVE ( 'NONE', #11615, #8207, #10160, .T. ) ;
#12957 = ADVANCED_FACE ( 'NONE', ( #11349 ), #5365, .F. ) ;
#12958 = EDGE_LOOP ( 'NONE', ( #6788, #9731 ) ) ;
#12959 = EDGE_LOOP ( 'NONE', ( #3483, #14369, #12141, #14474 ) ) ;
#12960 = ORIENTED_EDGE ( 'NONE', *, *, #11734, .T. ) ;
#12961 = DIRECTION ( 'NONE',  ( -0.000000000000000000, -1.000000000000000000, -0.000000000000000000 ) ) ;
#12962 = DIRECTION ( 'NONE',  ( 1.000000000000000000, 0.000000000000000000, 0.000000000000000000 ) ) ;
#12963 = CARTESIAN_POINT ( 'NONE',  ( 0.3725000000000000533, 0.1749999999999999889, -0.4124999999999999778 ) ) ;
#12964 = EDGE_CURVE ( 'NONE', #6953, #10875, #11511, .T. ) ;
#12965 = DIRECTION ( 'NONE',  ( 0.000000000000000000, 0.000000000000000000, -1.000000000000000000 ) ) ;
#12966 = EDGE_LOOP ( 'NONE', ( #7360, #6030, #10868, #11786 ) ) ;
#12967 = CIRCLE ( 'NONE', #9315, 0.5000000000000002220 ) ;
#12968 = CARTESIAN_POINT ( 'NONE',  ( 2.774999999999999911, 1.575000000000000178, -2.360000000000016751 ) ) ;
#12969 = CARTESIAN_POINT ( 'NONE',  ( 1.936238515863016874, 0.2305039212132600213, 0.4121290732901491394 ) ) ;
#12970 = CARTESIAN_POINT ( 'NONE',  ( 3.102108017520305072, 0.6812791890164020536, -0.3964255093850734268 ) ) ;
#12971 = ADVANCED_FACE ( 'NONE', ( #8155 ), #13940, .F. ) ;
#12972 = CARTESIAN_POINT ( 'NONE',  ( 1.813794508430887964, 0.1486894511058793333, -0.4139507449637808145 ) ) ;
#12973 = VECTOR ( 'NONE', #12716, 39.37007874015748854 ) ;
#12974 = ORIENTED_EDGE ( 'NONE', *, *, #12470, .T. ) ;
#12976 = EDGE_LOOP ( 'NONE', ( #9352, #4146, #5960, #7514 ) ) ;
#12975 = DIRECTION ( 'NONE',  ( -0.000000000000000000, 1.000000000000000000, 4.591341165821852610E-16 ) ) ;
#12977 = ORIENTED_EDGE ( 'NONE', *, *, #4009, .T. ) ;
#12978 = CARTESIAN_POINT ( 'NONE',  ( 3.874999999999999556, 3.170500000000000096, 1.509999999999999787 ) ) ;
#12979 = EDGE_LOOP ( 'NONE', ( #3608, #6234, #2487, #10281 ) ) ;
#12980 = CARTESIAN_POINT ( 'NONE',  ( 2.774999999999999911, -1.679378605318041950, 1.679378605318059048 ) ) ;
#12981 = CARTESIAN_POINT ( 'NONE',  ( 8.475037399843312613, 0.9969999999999998863, 0.3802960819231170908 ) ) ;
#12982 = VERTEX_POINT ( 'NONE', #14797 ) ;
#12983 = CARTESIAN_POINT ( 'NONE',  ( 0.2249147617188371751, 1.559103846021539619, -0.3723417112827391295 ) ) ;
#12984 = DIRECTION ( 'NONE',  ( -0.000000000000000000, 1.000000000000000000, -0.000000000000000000 ) ) ;
#12985 = EDGE_CURVE ( 'NONE', #2425, #11436, #13125, .T. ) ;
#12986 = CARTESIAN_POINT ( 'NONE',  ( 3.773638191489542493, 1.892500311876669894, 0.7431788962619894079 ) ) ;
#12987 = VECTOR ( 'NONE', #3415, 39.37007874015748143 ) ;
#12988 = DIRECTION ( 'NONE',  ( 0.8660254037844387076, 0.000000000000000000, -0.4999999999999998890 ) ) ;
#12989 = EDGE_CURVE ( 'NONE', #4487, #9683, #12721, .T. ) ;
#12990 = DIRECTION ( 'NONE',  ( 0.000000000000000000, 1.000000000000000000, 0.000000000000000000 ) ) ;
#12991 = DIRECTION ( 'NONE',  ( -1.000000000000000000, -0.000000000000000000, -0.000000000000000000 ) ) ;
#12992 = FACE_BOUND ( 'NONE', #13122, .T. ) ;
#12993 = CARTESIAN_POINT ( 'NONE',  ( 3.992641157495913085, 1.749621749097510115, 0.7883586273357179319 ) ) ;
#12994 = VERTEX_POINT ( 'NONE', #13782 ) ;
#12995 = CARTESIAN_POINT ( 'NONE',  ( 0.6570838759023790443, -0.3876519068829718528, 0.5130260770772535617 ) ) ;
#12997 = ORIENTED_EDGE ( 'NONE', *, *, #8583, .T. ) ;
#12996 = DIRECTION ( 'NONE',  ( 1.000000000000000000, 0.000000000000000000, 0.000000000000000000 ) ) ;
#12998 = EDGE_LOOP ( 'NONE', ( #5782, #4399, #7211, #4043, #9775 ) ) ;
#12999 = CARTESIAN_POINT ( 'NONE',  ( 6.215861650065340527, 3.673940397442060361E-16, -3.000000000000000444 ) ) ;
#13000 = CARTESIAN_POINT ( 'NONE',  ( 3.241046123363278131, 0.7391609583210639878, 0.4542225123818745547 ) ) ;
#13001 = ORIENTED_EDGE ( 'NONE', *, *, #6524, .T. ) ;
#13002 = CARTESIAN_POINT ( 'NONE',  ( 0.9672769954795885639, -0.4829975555521403008, -0.4081482409674996870 ) ) ;
#13003 = AXIS2_PLACEMENT_3D ( 'NONE', #8519, #5286, #294 ) ;
#13004 = EDGE_CURVE ( 'NONE', #11380, #14026, #7994, .T. ) ;
#13005 = EDGE_CURVE ( 'NONE', #11969, #355, #12491, .T. ) ;
#13006 = DIRECTION ( 'NONE',  ( -1.000000000000000000, -0.000000000000000000, -0.000000000000000000 ) ) ;
#13007 = CARTESIAN_POINT ( 'NONE',  ( 2.774999999999999911, 0.000000000000000000, 0.000000000000000000 ) ) ;
#13008 = ORIENTED_EDGE ( 'NONE', *, *, #13511, .T. ) ;
#13009 = CARTESIAN_POINT ( 'NONE',  ( 0.6842449982442055934, -0.4393369316438217598, 0.4560737988759885897 ) ) ;
#13010 = FACE_OUTER_BOUND ( 'NONE', #13507, .T. ) ;
#13011 = DIRECTION ( 'NONE',  ( 0.000000000000000000, 0.000000000000000000, -1.000000000000000000 ) ) ;
#13012 = ORIENTED_EDGE ( 'NONE', *, *, #1734, .T. ) ;
#13013 = DIRECTION ( 'NONE',  ( -1.000000000000000000, -0.000000000000000000, -0.000000000000000000 ) ) ;
#13014 = ORIENTED_EDGE ( 'NONE', *, *, #11576, .T. ) ;
#13015 = CARTESIAN_POINT ( 'NONE',  ( 2.124999999999999556, 1.679378605318042395, -1.679378605318058604 ) ) ;
#13016 = ORIENTED_EDGE ( 'NONE', *, *, #13511, .F. ) ;
#13017 =( BOUNDED_CURVE ( )  B_SPLINE_CURVE ( 3, ( #6837, #2615, #4919, #7215 ),
 .UNSPECIFIED., .F., .T. ) 
 B_SPLINE_CURVE_WITH_KNOTS ( ( 4, 4 ),
 ( 0.7853981633974534970, 1.570796326794896336 ),
 .UNSPECIFIED. ) 
 CURVE ( )  GEOMETRIC_REPRESENTATION_ITEM ( )  RATIONAL_B_SPLINE_CURVE ( ( 1.000000000000000000, 0.9492530216741918991, 0.9492530216741918991, 1.000000000000000000 ) ) 
 REPRESENTATION_ITEM ( '' )  );
#13018 = CARTESIAN_POINT ( 'NONE',  ( 3.944129661530210385, 0.000000000000000000, 0.000000000000000000 ) ) ;
#13019 = AXIS2_PLACEMENT_3D ( 'NONE', #15051, #4576, #9248 ) ;
#13020 = CARTESIAN_POINT ( 'NONE',  ( 1.261796151055236015, -0.4301078242393568951, -0.4222829664661058580 ) ) ;
#13021 = ADVANCED_FACE ( 'NONE', ( #10438 ), #9304, .F. ) ;
#13022 = CARTESIAN_POINT ( 'NONE',  ( 3.426491571325181340, 0.000000000000000000, 0.000000000000000000 ) ) ;
#13023 = FACE_OUTER_BOUND ( 'NONE', #9461, .T. ) ;
#13024 = AXIS2_PLACEMENT_3D ( 'NONE', #2520, #8419, #1280 ) ;
#13025 = ORIENTED_EDGE ( 'NONE', *, *, #11233, .T. ) ;
#13026 = ORIENTED_EDGE ( 'NONE', *, *, #12770, .F. ) ;
#13027 = ORIENTED_EDGE ( 'NONE', *, *, #4633, .F. ) ;
#13028 = CARTESIAN_POINT ( 'NONE',  ( 3.426491571325181340, 2.056041051583894497, 0.5999481385562638325 ) ) ;
#13029 = CARTESIAN_POINT ( 'NONE',  ( 2.742999999999998995, -1.679378605318059048, -1.416878605318056872 ) ) ;
#13030 = CARTESIAN_POINT ( 'NONE',  ( 0.8369793835502591373, -0.4830000000000001514, -0.4162690208630439037 ) ) ;
#13031 = LINE ( 'NONE', #6942, #10723 ) ;
#13032 = VERTEX_POINT ( 'NONE', #13712 ) ;
#13033 = CARTESIAN_POINT ( 'NONE',  ( 3.876560711617219379, 2.750000000000000000, 0.000000000000000000 ) ) ;
#13034 = EDGE_CURVE ( 'NONE', #13813, #11971, #3365, .T. ) ;
#13035 = CARTESIAN_POINT ( 'NONE',  ( 3.015109087180224771E-17, -0.4844395604395604904, 0.000000000000000000 ) ) ;
#13036 = CONICAL_SURFACE ( 'NONE', #11585, 0.2624999999999852451, 0.7853981633974428389 ) ;
#13037 = DIRECTION ( 'NONE',  ( 0.000000000000000000, 1.000000000000000000, -0.000000000000000000 ) ) ;
#13038 = AXIS2_PLACEMENT_3D ( 'NONE', #9507, #6908, #8210 ) ;
#13039 = VERTEX_POINT ( 'NONE', #10290 ) ;
#13041 = ORIENTED_EDGE ( 'NONE', *, *, #2231, .F. ) ;
#13040 = DIRECTION ( 'NONE',  ( -0.000000000000000000, -1.000000000000000000, -0.000000000000000000 ) ) ;
#13042 = AXIS2_PLACEMENT_3D ( 'NONE', #7323, #11975, #314 ) ;
#13043 = EDGE_LOOP ( 'NONE', ( #13103, #7469, #2115, #10565 ) ) ;
#13044 = DIRECTION ( 'NONE',  ( -0.000000000000000000, -1.000000000000000000, -0.000000000000000000 ) ) ;
#13045 = EDGE_LOOP ( 'NONE', ( #4459, #5265, #14423, #12683 ) ) ;
#13046 = PRODUCT_DEFINITION_FORMATION_WITH_SPECIFIED_SOURCE ( 'ANY', '', #12267, .NOT_KNOWN. ) ;
#13047 = DIRECTION ( 'NONE',  ( 0.000000000000000000, 0.000000000000000000, 1.000000000000000000 ) ) ;
#13048 = CARTESIAN_POINT ( 'NONE',  ( 3.874999999999999556, 2.407999999999999918, -1.320000000000000062 ) ) ;
#13049 = PLANE ( 'NONE',  #12095 ) ;
#13050 = ORIENTED_EDGE ( 'NONE', *, *, #11963, .T. ) ;
#13051 = FACE_OUTER_BOUND ( 'NONE', #6880, .T. ) ;
#13052 = DIRECTION ( 'NONE',  ( 0.000000000000000000, 0.000000000000000000, 1.000000000000000000 ) ) ;
#13053 = EDGE_CURVE ( 'NONE', #4833, #3395, #7970, .T. ) ;
#13054 = EDGE_CURVE ( 'NONE', #2564, #5506, #2173, .T. ) ;
#13055 = DIRECTION ( 'NONE',  ( -1.000000000000000000, -0.000000000000000000, -0.000000000000000000 ) ) ;
#13056 = EDGE_CURVE ( 'NONE', #11912, #12552, #1398, .T. ) ;
#13057 = CONICAL_SURFACE ( 'NONE', #6473, 0.1899999999999996136, 0.7853981633974530530 ) ;
#13058 = CARTESIAN_POINT ( 'NONE',  ( 6.826491571325181695, 0.000000000000000000, 0.000000000000000000 ) ) ;
#13059 = CIRCLE ( 'NONE', #8672, 0.5000000000000000000 ) ;
#13060 = VECTOR ( 'NONE', #14230, 39.37007874015748143 ) ;
#13061 = DIRECTION ( 'NONE',  ( 1.000000000000000000, 0.000000000000000000, 0.000000000000000000 ) ) ;
#13062 = EDGE_CURVE ( 'NONE', #1193, #7063, #1886, .T. ) ;
#13063 = DIRECTION ( 'NONE',  ( 0.7071067811865450192, 8.659560562354962440E-17, 0.7071067811865499042 ) ) ;
#13064 = FACE_BOUND ( 'NONE', #1016, .T. ) ;
#13065 = ADVANCED_FACE ( 'NONE', ( #14018 ), #2633, .F. ) ;
#13066 = VERTEX_POINT ( 'NONE', #3637 ) ;
#13067 = DIRECTION ( 'NONE',  ( -0.4938181170261085051, 0.000000000000000000, 0.8695652173913058780 ) ) ;
#13069 = EDGE_LOOP ( 'NONE', ( #9718, #11697 ) ) ;
#13068 = FACE_OUTER_BOUND ( 'NONE', #4730, .T. ) ;
#13070 = ORIENTED_EDGE ( 'NONE', *, *, #3906, .T. ) ;
#13071 = DIRECTION ( 'NONE',  ( 0.000000000000000000, 0.7071067811865430208, 0.7071067811865520136 ) ) ;
#13072 = AXIS2_PLACEMENT_3D ( 'NONE', #8448, #11958, #2626 ) ;
#13073 = DIRECTION ( 'NONE',  ( 0.000000000000000000, 0.000000000000000000, -1.000000000000000000 ) ) ;
#13074 = CARTESIAN_POINT ( 'NONE',  ( 2.854443715606396648, 0.5365358177142092178, 0.4001101571913798782 ) ) ;
#13075 = ORIENTED_EDGE ( 'NONE', *, *, #10083, .F. ) ;
#13076 = DIRECTION ( 'NONE',  ( -1.000000000000000000, 0.000000000000000000, 0.000000000000000000 ) ) ;
#13077 = AXIS2_PLACEMENT_3D ( 'NONE', #2910, #12233, #3359 ) ;
#13078 = TOROIDAL_SURFACE ( 'NONE', #3076, 0.5849999999999996314, 0.1000000000000000056 ) ;
#13079 = DIRECTION ( 'NONE',  ( -1.000000000000000000, -0.000000000000000000, -0.000000000000000000 ) ) ;
#13080 = DIRECTION ( 'NONE',  ( -0.000000000000000000, 1.000000000000000000, -0.000000000000000000 ) ) ;
#13081 = ADVANCED_FACE ( 'NONE', ( #9458 ), #7049, .F. ) ;
#13082 = ORIENTED_EDGE ( 'NONE', *, *, #10775, .F. ) ;
#13083 = AXIS2_PLACEMENT_3D ( 'NONE', #2379, #5268, #13358 ) ;
#13084 = CARTESIAN_POINT ( 'NONE',  ( 2.124999999999999556, 2.399999999999999911, -0.7000000000000009548 ) ) ;
#13085 = CARTESIAN_POINT ( 'NONE',  ( 0.000000000000000000, 0.000000000000000000, -0.4850000000000000422 ) ) ;
#13086 = AXIS2_PLACEMENT_3D ( 'NONE', #6126, #14286, #5967 ) ;
#13087 = FACE_OUTER_BOUND ( 'NONE', #12006, .T. ) ;
#13088 = ADVANCED_FACE ( 'NONE', ( #8321 ), #2398, .F. ) ;
#13089 = ORIENTED_EDGE ( 'NONE', *, *, #6175, .F. ) ;
#13090 = DIRECTION ( 'NONE',  ( 0.000000000000000000, 0.000000000000000000, -1.000000000000000000 ) ) ;
#13091 = CARTESIAN_POINT ( 'NONE',  ( 6.208491571325183145, -1.679378605318048390, 1.679378605318054163 ) ) ;
#13092 = ORIENTED_EDGE ( 'NONE', *, *, #8122, .T. ) ;
#13093 = EDGE_CURVE ( 'NONE', #7368, #14441, #11681, .T. ) ;
#13094 = CARTESIAN_POINT ( 'NONE',  ( 0.2849999999999999756, 5.750000000000000000, -0.4108223460329293864 ) ) ;
#13095 = VERTEX_POINT ( 'NONE', #2406 ) ;
#13096 = AXIS2_PLACEMENT_3D ( 'NONE', #8409, #13891, #12905 ) ;
#13097 = CARTESIAN_POINT ( 'NONE',  ( 1.503855556006640448, -0.3209522984519411759, -0.4787591023162905413 ) ) ;
#13098 = DIRECTION ( 'NONE',  ( 0.000000000000000000, 0.000000000000000000, 1.000000000000000000 ) ) ;
#13099 = FACE_OUTER_BOUND ( 'NONE', #6423, .T. ) ;
#13100 = DIRECTION ( 'NONE',  ( 0.000000000000000000, 0.000000000000000000, -1.000000000000000000 ) ) ;
#13101 = CIRCLE ( 'NONE', #3841, 0.05999999999999990757 ) ;
#13102 =( BOUNDED_CURVE ( )  B_SPLINE_CURVE ( 3, ( #5352, #10936, #3833, #5195 ),
 .UNSPECIFIED., .F., .F. ) 
 B_SPLINE_CURVE_WITH_KNOTS ( ( 4, 4 ),
 ( 0.7853981633974463916, 1.570796326794896558 ),
 .UNSPECIFIED. ) 
 CURVE ( )  GEOMETRIC_REPRESENTATION_ITEM ( )  RATIONAL_B_SPLINE_CURVE ( ( 1.000000000000000000, 0.9492530216741910110, 0.9492530216741910110, 1.000000000000000000 ) ) 
 REPRESENTATION_ITEM ( '' )  );
#13103 = ORIENTED_EDGE ( 'NONE', *, *, #3950, .T. ) ;
#13104 = ORIENTED_EDGE ( 'NONE', *, *, #9048, .F. ) ;
#13105 = VERTEX_POINT ( 'NONE', #303 ) ;
#13106 = ADVANCED_FACE ( 'NONE', ( #4865 ), #4594, .F. ) ;
#13107 = CARTESIAN_POINT ( 'NONE',  ( 3.426491571325181340, 0.6999999999999599876, -2.400000000000011458 ) ) ;
#13108 = CARTESIAN_POINT ( 'NONE',  ( 3.874999999999999556, 3.137999999999999901, -1.097499999999998810 ) ) ;
#13109 = AXIS2_PLACEMENT_3D ( 'NONE', #13198, #2735, #407 ) ;
#13110 = DIRECTION ( 'NONE',  ( 0.000000000000000000, 1.000000000000000000, 0.000000000000000000 ) ) ;
#13111 = DIRECTION ( 'NONE',  ( 1.000000000000000000, 0.000000000000000000, 0.000000000000000000 ) ) ;
#13112 = CARTESIAN_POINT ( 'NONE',  ( 3.817400053824495654, 1.897687926027022520, -0.4968051402951919604 ) ) ;
#13113 = AXIS2_PLACEMENT_3D ( 'NONE', #9686, #1624, #14256 ) ;
#13114 = CARTESIAN_POINT ( 'NONE',  ( 1.542522555076119239, 0.03620193991696377817, 0.4782129582616606589 ) ) ;
#13115 = DIRECTION ( 'NONE',  ( 0.000000000000000000, -0.7071067811865366926, 0.7071067811865584529 ) ) ;
#13116 = AXIS2_PLACEMENT_3D ( 'NONE', #4435, #6963, #13676 ) ;
#13117 = EDGE_LOOP ( 'NONE', ( #12249, #13887, #13725, #7116 ) ) ;
#13119 = VERTEX_POINT ( 'NONE', #11746 ) ;
#13118 = CARTESIAN_POINT ( 'NONE',  ( 3.874999999999999556, 2.782000000000000917, -1.509999999999999787 ) ) ;
#13120 = VERTEX_POINT ( 'NONE', #7236 ) ;
#13121 = DIRECTION ( 'NONE',  ( -0.000000000000000000, -1.000000000000000000, -0.000000000000000000 ) ) ;
#13122 = EDGE_LOOP ( 'NONE', ( #15133, #9695 ) ) ;
#13123 = EDGE_CURVE ( 'NONE', #8716, #14113, #6308, .T. ) ;
#13124 = DIRECTION ( 'NONE',  ( -1.000000000000000000, -0.000000000000000000, -0.000000000000000000 ) ) ;
#13125 = CIRCLE ( 'NONE', #5087, 0.2625000000000000111 ) ;
#13126 = APPLICATION_PROTOCOL_DEFINITION ( 'draft international standard', 'automotive_design', 1998, #9200 ) ;
#13127 = CARTESIAN_POINT ( 'NONE',  ( 2.630032447663273043, 0.7405933021011417150, 0.4628526490443040653 ) ) ;
#13128 = ORIENTED_EDGE ( 'NONE', *, *, #6387, .T. ) ;
#13129 = CARTESIAN_POINT ( 'NONE',  ( 0.6180000000000012150, 0.000000000000000000, 0.000000000000000000 ) ) ;
#13130 = DIRECTION ( 'NONE',  ( 0.000000000000000000, 0.000000000000000000, -1.000000000000000000 ) ) ;
#13131 = VECTOR ( 'NONE', #5833, 39.37007874015748143 ) ;
#13132 = CARTESIAN_POINT ( 'NONE',  ( 1.564978703518703940, 0.000000000000000000, -0.4193347797797316034 ) ) ;
#13133 = VECTOR ( 'NONE', #13954, 39.37007874015748143 ) ;
#13134 = DIRECTION ( 'NONE',  ( -1.000000000000000000, -0.000000000000000000, -0.000000000000000000 ) ) ;
#13135 = AXIS2_PLACEMENT_3D ( 'NONE', #10102, #7646, #14686 ) ;
#13136 = CARTESIAN_POINT ( 'NONE',  ( 0.8369029794110903753, -0.4829999991353697841, -0.4161243967669134847 ) ) ;
#13137 = CARTESIAN_POINT ( 'NONE',  ( 3.426491571325181340, 1.575000000000000178, -2.360000000000018971 ) ) ;
#13138 = ADVANCED_FACE ( 'NONE', ( #14177 ), #1472, .F. ) ;
#13139 = CARTESIAN_POINT ( 'NONE',  ( 6.794491571325179891, -1.679378605318047946, -1.304378605318053053 ) ) ;
#13140 = ADVANCED_FACE ( 'NONE', ( #1318 ), #5574, .F. ) ;
#13141 = ORIENTED_EDGE ( 'NONE', *, *, #8944, .F. ) ;
#13142 = ADVANCED_FACE ( 'NONE', ( #239 ), #14350, .T. ) ;
#13143 = DIRECTION ( 'NONE',  ( 0.8695652173913053229, 0.000000000000000000, 0.4938181170261089492 ) ) ;
#13145 = ORIENTED_EDGE ( 'NONE', *, *, #13461, .T. ) ;
#13144 = DIRECTION ( 'NONE',  ( 0.000000000000000000, 0.000000000000000000, 1.000000000000000000 ) ) ;
#13146 = VECTOR ( 'NONE', #1925, 39.37007874015748854 ) ;
#13147 = ORIENTED_EDGE ( 'NONE', *, *, #7639, .F. ) ;
#13148 = VECTOR ( 'NONE', #4443, 39.37007874015748854 ) ;
#13149 = CONICAL_SURFACE ( 'NONE', #12915, 1.350000000000000089, 0.2094395102393122321 ) ;
#13150 = DIRECTION ( 'NONE',  ( -1.000000000000000000, -0.000000000000000000, -0.000000000000000000 ) ) ;
#13151 = DIRECTION ( 'NONE',  ( 0.000000000000000000, 0.000000000000000000, -1.000000000000000000 ) ) ;
#13152 = ORIENTED_EDGE ( 'NONE', *, *, #6820, .T. ) ;
#13153 = VECTOR ( 'NONE', #151, 39.37007874015748143 ) ;
#13154 = CARTESIAN_POINT ( 'NONE',  ( 0.09500000000000431710, 1.679378605318035733, -1.679378605318065487 ) ) ;
#13155 = EDGE_CURVE ( 'NONE', #1024, #14149, #9676, .T. ) ;
#13156 = CARTESIAN_POINT ( 'NONE',  ( 0.6653223438648792065, 0.01646029051545267255, 0.4725272431374084592 ) ) ;
#13157 = PLANE ( 'NONE',  #4627 ) ;
#13158 = ORIENTED_EDGE ( 'NONE', *, *, #10381, .F. ) ;
#13159 = AXIS2_PLACEMENT_3D ( 'NONE', #380, #14466, #5453 ) ;
#13160 = CARTESIAN_POINT ( 'NONE',  ( 3.875000000000000000, 3.137999999999999901, 0.000000000000000000 ) ) ;
#13161 = CARTESIAN_POINT ( 'NONE',  ( 0.2849999999999998090, 4.529999999999999361, -0.4108223460329292198 ) ) ;
#13162 =( NAMED_UNIT ( * ) PLANE_ANGLE_UNIT ( ) SI_UNIT ( $, .RADIAN. ) );
#13163 = VERTEX_POINT ( 'NONE', #4782 ) ;
#13164 = CONICAL_SURFACE ( 'NONE', #1190, 1.000000000000000000, 0.7853981633974477239 ) ;
#13165 = DIRECTION ( 'NONE',  ( -1.000000000000000000, -0.000000000000000000, -0.000000000000000000 ) ) ;
#13166 = CARTESIAN_POINT ( 'NONE',  ( -0.3724999999999999423, 0.1749999999999999889, 0.4124999999999999778 ) ) ;
#13167 = VERTEX_POINT ( 'NONE', #14326 ) ;
#13168 = CARTESIAN_POINT ( 'NONE',  ( 0.7058998964907862161, -0.05999999999999994227, 0.4900296624789436950 ) ) ;
#13169 = VERTEX_POINT ( 'NONE', #14100 ) ;
#13170 = LINE ( 'NONE', #10602, #5122 ) ;
#13171 = AXIS2_PLACEMENT_3D ( 'NONE', #1146, #8062, #4688 ) ;
#13172 = DIRECTION ( 'NONE',  ( 0.000000000000000000, 0.000000000000000000, -1.000000000000000000 ) ) ;
#13173 = ADVANCED_FACE ( 'NONE', ( #6005 ), #10670, .F. ) ;
#13174 = CONICAL_SURFACE ( 'NONE', #3180, 0.07000000000000047851, 0.7853981633974297383 ) ;
#13175 = CARTESIAN_POINT ( 'NONE',  ( 3.426491571325181340, 0.000000000000000000, 0.000000000000000000 ) ) ;
#13176 = DIRECTION ( 'NONE',  ( -0.7071067811865400232, 0.000000000000000000, 0.7071067811865551223 ) ) ;
#13177 = ADVANCED_FACE ( 'NONE', ( #3782 ), #8026, .F. ) ;
#13178 = CARTESIAN_POINT ( 'NONE',  ( 0.000000000000000000, 1.653273178848927113E-16, -1.350000000000000089 ) ) ;
#13179 = ORIENTED_EDGE ( 'NONE', *, *, #2904, .F. ) ;
#13180 = ORIENTED_EDGE ( 'NONE', *, *, #9118, .T. ) ;
#13181 = EDGE_LOOP ( 'NONE', ( #1142, #6783, #1561, #9646 ) ) ;
#13182 = CARTESIAN_POINT ( 'NONE',  ( 0.6180000000000012150, 3.673940397442060361E-16, -3.000000000000000444 ) ) ;
#13183 = DIRECTION ( 'NONE',  ( -1.000000000000000000, -0.000000000000000000, -0.000000000000000000 ) ) ;
#13184 = DIRECTION ( 'NONE',  ( 0.000000000000000000, 0.000000000000000000, -1.000000000000000000 ) ) ;
#13185 = LINE ( 'NONE', #2723, #6085 ) ;
#13186 = CARTESIAN_POINT ( 'NONE',  ( 3.426491571325181340, 1.958272580636415405, -0.6732367908064789130 ) ) ;
#13187 = CARTESIAN_POINT ( 'NONE',  ( 2.045923089166573394, 0.3299328314968411058, 0.4711027812264608761 ) ) ;
#13188 = SURFACE_STYLE_USAGE ( .BOTH. , #12403 ) ;
#13189 = ADVANCED_FACE ( 'NONE', ( #3932 ), #11184, .F. ) ;
#13190 = EDGE_CURVE ( 'NONE', #6615, #6953, #12398, .T. ) ;
#13191 = CARTESIAN_POINT ( 'NONE',  ( 4.456236641444369262, 1.708450350955834418, -0.5507572246836857088 ) ) ;
#13192 = EDGE_LOOP ( 'NONE', ( #8267, #4129, #9383, #12349, #351, #14806 ) ) ;
#13193 = VERTEX_POINT ( 'NONE', #13310 ) ;
#13194 = ORIENTED_EDGE ( 'NONE', *, *, #11715, .F. ) ;
#13195 = CIRCLE ( 'NONE', #7362, 0.06000000000000005329 ) ;
#13196 = CYLINDRICAL_SURFACE ( 'NONE', #4827, 0.1900000000000000577 ) ;
#13197 = DIMENSIONAL_EXPONENTS ( 1.000000000000000000, 0.000000000000000000, 0.000000000000000000, 0.000000000000000000, 0.000000000000000000, 0.000000000000000000, 0.000000000000000000 ) ;
#13198 = CARTESIAN_POINT ( 'NONE',  ( 0.06299999999999998657, 0.000000000000000000, 0.000000000000000000 ) ) ;
#13199 = CARTESIAN_POINT ( 'NONE',  ( 4.358578070590652942, 0.9918745563571595980, -0.1313582112852187400 ) ) ;
#13200 = FACE_OUTER_BOUND ( 'NONE', #5325, .T. ) ;
#13201 = ORIENTED_EDGE ( 'NONE', *, *, #12876, .T. ) ;
#13202 = CARTESIAN_POINT ( 'NONE',  ( 3.874999999999999556, 3.535499999999999421, -1.130000000000000560 ) ) ;
#13203 = DIRECTION ( 'NONE',  ( 0.000000000000000000, 1.000000000000000000, 0.000000000000000000 ) ) ;
#13204 = CARTESIAN_POINT ( 'NONE',  ( 3.444319122601930972E-17, 0.000000000000000000, 0.2812500000000000555 ) ) ;
#13205 = CARTESIAN_POINT ( 'NONE',  ( 6.826491571325181695, -1.679378605318047946, -1.679378605318053497 ) ) ;
#13206 = VECTOR ( 'NONE', #11268, 39.37007874015748854 ) ;
#13207 = CARTESIAN_POINT ( 'NONE',  ( 0.000000000000000000, 1.159999999999999698, 0.000000000000000000 ) ) ;
#13208 = DIRECTION ( 'NONE',  ( -1.000000000000000000, -0.000000000000000000, 0.000000000000000000 ) ) ;
#13209 = CARTESIAN_POINT ( 'NONE',  ( 3.527413420661385413, 1.933330931508713268, 0.6651649055560091561 ) ) ;
#13210 = CARTESIAN_POINT ( 'NONE',  ( 2.774999999999999911, 0.000000000000000000, 0.000000000000000000 ) ) ;
#13211 = EDGE_LOOP ( 'NONE', ( #7102, #1202, #809, #6011 ) ) ;
#13212 = CARTESIAN_POINT ( 'NONE',  ( 0.6583797813917271480, -0.3800069445035944571, 0.5137833636068753762 ) ) ;
#13214 = VERTEX_POINT ( 'NONE', #12105 ) ;
#13213 = CARTESIAN_POINT ( 'NONE',  ( 2.774999999999999911, -0.9799999999999990941, -2.359999999999999876 ) ) ;
#13215 = ORIENTED_EDGE ( 'NONE', *, *, #9207, .F. ) ;
#13216 = FACE_OUTER_BOUND ( 'NONE', #7887, .T. ) ;
#13217 = CARTESIAN_POINT ( 'NONE',  ( 3.390179639970223313, 0.6913388717410868800, -0.3921396980529558429 ) ) ;
#13218 = EDGE_LOOP ( 'NONE', ( #13675, #7610, #3336, #13141 ) ) ;
#13219 = AXIS2_PLACEMENT_3D ( 'NONE', #8758, #2792, #1405 ) ;
#13220 = DIRECTION ( 'NONE',  ( 0.000000000000000000, 0.000000000000000000, 1.000000000000000000 ) ) ;
#13221 = ADVANCED_FACE ( 'NONE', ( #10049 ), #8829, .F. ) ;
#13222 = CARTESIAN_POINT ( 'NONE',  ( 0.6592137334438901153, 0.0006300111355865889223, 0.4885243083254864338 ) ) ;
#13223 = CARTESIAN_POINT ( 'NONE',  ( 2.774999999999999911, -3.360000000000016751, -0.9799999999999434719 ) ) ;
#13224 = VERTEX_POINT ( 'NONE', #605 ) ;
#13225 = CARTESIAN_POINT ( 'NONE',  ( 2.414213562373087374, 0.1427864376268978830, -0.4064941968476759038 ) ) ;
#13226 = DIRECTION ( 'NONE',  ( -1.000000000000000000, -0.000000000000000000, -0.000000000000000000 ) ) ;
#13227 = DIRECTION ( 'NONE',  ( -0.000000000000000000, -0.000000000000000000, -1.000000000000000000 ) ) ;
#13228 = VERTEX_POINT ( 'NONE', #5298 ) ;
#13229 = ADVANCED_FACE ( 'NONE', ( #2932 ), #179, .F. ) ;
#13230 = DIRECTION ( 'NONE',  ( -0.000000000000000000, -1.000000000000000000, -0.000000000000000000 ) ) ;
#13231 = VERTEX_POINT ( 'NONE', #14629 ) ;
#13232 = CARTESIAN_POINT ( 'NONE',  ( -0.7500000000000001110, 1.000000000000000222, 0.6614378277661475680 ) ) ;
#13233 = ORIENTED_EDGE ( 'NONE', *, *, #2625, .T. ) ;
#13234 = LENGTH_MEASURE_WITH_UNIT ( LENGTH_MEASURE( 0.02539999999999999897 ), #3489 );
#13235 = VECTOR ( 'NONE', #12241, 39.37007874015748143 ) ;
#13236 = DIRECTION ( 'NONE',  ( 0.000000000000000000, 0.000000000000000000, -1.000000000000000000 ) ) ;
#13237 = EDGE_CURVE ( 'NONE', #12566, #8835, #8824, .T. ) ;
#13238 = CARTESIAN_POINT ( 'NONE',  ( 8.475037399843314390, 0.9969999999999998863, -0.3802960819231170353 ) ) ;
#13239 = EDGE_CURVE ( 'NONE', #12151, #2908, #7667, .T. ) ;
#13240 = CARTESIAN_POINT ( 'NONE',  ( 0.06299999999999998657, 0.000000000000000000, 0.000000000000000000 ) ) ;
#13241 = AXIS2_PLACEMENT_3D ( 'NONE', #8280, #4906, #2524 ) ;
#13242 = DIRECTION ( 'NONE',  ( -1.000000000000000000, -0.000000000000000000, -0.000000000000000000 ) ) ;
#13243 = CARTESIAN_POINT ( 'NONE',  ( 1.328406321535847256, -0.06000000000013446660, -0.4812371988483638008 ) ) ;
#13244 = PRESENTATION_LAYER_ASSIGNMENT (  '', '', ( #7892 ) ) ;
#13245 = EDGE_CURVE ( 'NONE', #638, #14935, #13852, .T. ) ;
#13246 = VERTEX_POINT ( 'NONE', #12034 ) ;
#13247 = ORIENTED_EDGE ( 'NONE', *, *, #3442, .F. ) ;
#13248 = ORIENTED_EDGE ( 'NONE', *, *, #3934, .T. ) ;
#13249 = ADVANCED_FACE ( 'NONE', ( #8601 ), #2780, .T. ) ;
#13250 = DIRECTION ( 'NONE',  ( 0.7070715176384831935, 0.7070715176384805289, 0.009986885842351455114 ) ) ;
#13251 = CIRCLE ( 'NONE', #9375, 0.4070000000000022489 ) ;
#13252 = LINE ( 'NONE', #470, #8986 ) ;
#13253 = DIRECTION ( 'NONE',  ( 0.9999002670844990837, 0.000000000000000000, 0.01412288512831215773 ) ) ;
#13254 = CARTESIAN_POINT ( 'NONE',  ( 0.8999999999999999112, -0.6429999999999999050, -0.4300000000000014921 ) ) ;
#13255 = CARTESIAN_POINT ( 'NONE',  ( 6.826491571325181695, -1.679378605318048390, 1.679378605318054163 ) ) ;
#13256 = CARTESIAN_POINT ( 'NONE',  ( 4.559481147695757741, 1.797976069233882646, -0.3110169328516964038 ) ) ;
#13257 = CONICAL_SURFACE ( 'NONE', #9858, 0.2624999999999994560, 0.7853981633974446153 ) ;
#13258 = EDGE_CURVE ( 'NONE', #11127, #1772, #6799, .T. ) ;
#13259 = VECTOR ( 'NONE', #12788, 39.37007874015748143 ) ;
#13260 = CLOSED_SHELL ( 'NONE', ( #2571, #10773, #8430, #1762, #4711, #4421, #9638, #1928, #15067, #10444, #8330, #1464, #9440, #13707, #4206, #13138, #6180, #219, #2961, #11761, #11371 ) ) ;
#13261 = EDGE_LOOP ( 'NONE', ( #1890, #14829, #882, #14424 ) ) ;
#13262 = EDGE_LOOP ( 'NONE', ( #1705, #6866 ) ) ;
#13263 = ORIENTED_EDGE ( 'NONE', *, *, #7729, .F. ) ;
#13264 = DIRECTION ( 'NONE',  ( 0.000000000000000000, -1.224646799147354933E-16, 1.000000000000000000 ) ) ;
#13265 = CARTESIAN_POINT ( 'NONE',  ( 0.3724999999999997757, -0.6589999999999996971, -0.3725000000000000533 ) ) ;
#13266 = FACE_OUTER_BOUND ( 'NONE', #7687, .T. ) ;
#13267 = EDGE_CURVE ( 'NONE', #1703, #12765, #7980, .T. ) ;
#13268 = PRODUCT_CONTEXT ( 'NONE', #4706, 'mechanical' ) ;
#13269 = DIRECTION ( 'NONE',  ( 0.000000000000000000, -1.000000000000000000, -0.000000000000000000 ) ) ;
#13270 = ORIENTED_EDGE ( 'NONE', *, *, #7664, .F. ) ;
#13271 = VECTOR ( 'NONE', #6666, 39.37007874015748143 ) ;
#13272 = CARTESIAN_POINT ( 'NONE',  ( -0.2849999999999999756, 4.529999999999999361, -0.4108223460329293864 ) ) ;
#13273 = CARTESIAN_POINT ( 'NONE',  ( 3.426491571325181340, 0.7000000000000026201, 2.400000000000000355 ) ) ;
#13274 = AXIS2_PLACEMENT_3D ( 'NONE', #4734, #14906, #7339 ) ;
#13275 = CARTESIAN_POINT ( 'NONE',  ( 0.06299999999999994493, -1.679378605318047946, -1.679378605318053497 ) ) ;
#13276 = DIRECTION ( 'NONE',  ( 0.000000000000000000, 0.000000000000000000, -1.000000000000000000 ) ) ;
#13277 = FACE_OUTER_BOUND ( 'NONE', #14130, .T. ) ;
#13278 = DIRECTION ( 'NONE',  ( 0.000000000000000000, -1.000000000000000000, 0.000000000000000000 ) ) ;
#13279 = APPLICATION_CONTEXT ( 'automotive_design' ) ;
#13280 = VECTOR ( 'NONE', #11460, 39.37007874015748143 ) ;
#13281 = DIRECTION ( 'NONE',  ( 8.659560562354913137E-17, 0.7071067811865491270, -0.7071067811865459074 ) ) ;
#13282 = DIRECTION ( 'NONE',  ( -1.000000000000000000, -0.000000000000000000, -0.000000000000000000 ) ) ;
#13283 = ORIENTED_EDGE ( 'NONE', *, *, #5161, .F. ) ;
#13284 = PLANE ( 'NONE',  #15037 ) ;
#13286 = EDGE_LOOP ( 'NONE', ( #12951, #573 ) ) ;
#13285 = DIRECTION ( 'NONE',  ( 1.000000000000000000, 0.000000000000000000, 0.000000000000000000 ) ) ;
#13287 = ORIENTED_EDGE ( 'NONE', *, *, #13947, .T. ) ;
#13288 = CARTESIAN_POINT ( 'NONE',  ( 6.208491571325183145, 1.679378605318059492, 1.679378605318041506 ) ) ;
#13289 = ADVANCED_FACE ( 'NONE', ( #12472 ), #2148, .T. ) ;
#13290 = DIRECTION ( 'NONE',  ( -1.000000000000000000, -0.000000000000000000, -0.000000000000000000 ) ) ;
#13291 = ORIENTED_EDGE ( 'NONE', *, *, #4997, .T. ) ;
#13292 = CARTESIAN_POINT ( 'NONE',  ( 6.826491571325181695, -1.679378605318047946, -2.086378605318055968 ) ) ;
#13293 = DIRECTION ( 'NONE',  ( 0.7071067811865479058, 0.000000000000000000, -0.7071067811865472397 ) ) ;
#13294 = CIRCLE ( 'NONE', #10629, 0.3750000000000007772 ) ;
#13295 = AXIS2_PLACEMENT_3D ( 'NONE', #6558, #1791, #11136 ) ;
#13296 = CARTESIAN_POINT ( 'NONE',  ( 0.6742332106589076224, -0.02527202722326431922, 0.4798232997575394010 ) ) ;
#13297 = CARTESIAN_POINT ( 'NONE',  ( 2.124999999999999556, 2.296212748401287479E-16, 1.875000000000000000 ) ) ;
#13298 = ORIENTED_EDGE ( 'NONE', *, *, #9243, .F. ) ;
#13299 = CARTESIAN_POINT ( 'NONE',  ( 6.794491571325179891, 1.679378605318035733, -1.679378605318065487 ) ) ;
#13300 = DIRECTION ( 'NONE',  ( 0.000000000000000000, 1.000000000000000000, -0.000000000000000000 ) ) ;
#13301 = DIRECTION ( 'NONE',  ( 0.000000000000000000, 0.000000000000000000, -1.000000000000000000 ) ) ;
#13302 = AXIS2_PLACEMENT_3D ( 'NONE', #3208, #8110, #1893 ) ;
#13303 = CARTESIAN_POINT ( 'NONE',  ( 6.176491571325181340, 1.679378605318035733, -1.679378605318065487 ) ) ;
#13304 = VERTEX_POINT ( 'NONE', #7894 ) ;
#13305 = AXIS2_PLACEMENT_3D ( 'NONE', #12641, #6854, #12719 ) ;
#13306 = DIRECTION ( 'NONE',  ( 0.000000000000000000, 0.000000000000000000, 1.000000000000000000 ) ) ;
#13307 = ORIENTED_EDGE ( 'NONE', *, *, #6820, .F. ) ;
#13308 = PLANE ( 'NONE',  #2175 ) ;
#13309 = VECTOR ( 'NONE', #12864, 39.37007874015748143 ) ;
#13310 = CARTESIAN_POINT ( 'NONE',  ( 2.124999999999999556, -2.360000000000016751, -1.574999999999999956 ) ) ;
#13311 = CARTESIAN_POINT ( 'NONE',  ( 2.124999999999999556, 3.360000000000016751, 0.9799999999999461364 ) ) ;
#13312 = AXIS2_PLACEMENT_3D ( 'NONE', #12000, #2816, #345 ) ;
#13313 = AXIS2_PLACEMENT_3D ( 'NONE', #14789, #6686, #14865 ) ;
#13314 = LINE ( 'NONE', #2635, #15025 ) ;
#13315 = CARTESIAN_POINT ( 'NONE',  ( 0.000000000000000000, 0.1749999999999999889, 0.000000000000000000 ) ) ;
#13316 = VERTEX_POINT ( 'NONE', #10124 ) ;
#13317 = ORIENTED_EDGE ( 'NONE', *, *, #10412, .F. ) ;
#13318 = EDGE_CURVE ( 'NONE', #8947, #1719, #5757, .T. ) ;
#13319 = ORIENTED_EDGE ( 'NONE', *, *, #5525, .F. ) ;
#13320 = EDGE_CURVE ( 'NONE', #251, #7417, #2637, .T. ) ;
#13321 = VECTOR ( 'NONE', #6598, 39.37007874015748143 ) ;
#13322 = CARTESIAN_POINT ( 'NONE',  ( 8.559253539154886070, 0.8718469098602883438, -0.3109429831200917205 ) ) ;
#13323 = ADVANCED_FACE ( 'NONE', ( #14854 ), #2574, .T. ) ;
#13324 = LINE ( 'NONE', #2720, #8496 ) ;
#13325 = AXIS2_PLACEMENT_3D ( 'NONE', #13704, #6767, #2163 ) ;
#13326 = LINE ( 'NONE', #10136, #7383 ) ;
#13327 = CARTESIAN_POINT ( 'NONE',  ( 0.7058998964907862161, -0.3830000000000000071, 0.4900296624789436950 ) ) ;
#13328 = CARTESIAN_POINT ( 'NONE',  ( 0.000000000000000000, 5.750000000000000000, -0.4108223460329293864 ) ) ;
#13329 = EDGE_CURVE ( 'NONE', #11602, #11005, #2320, .T. ) ;
#13330 = ADVANCED_FACE ( 'NONE', ( #8979 ), #8896, .F. ) ;
#13331 = CARTESIAN_POINT ( 'NONE',  ( 0.8999999999999998002, 0.1549999999999996103, -0.3799999999999999489 ) ) ;
#13332 = CONICAL_SURFACE ( 'NONE', #10911, 0.06999999999999829969, 0.7853981633974298493 ) ;
#13333 = DIRECTION ( 'NONE',  ( -1.655665450705613915E-16, 0.000000000000000000, -1.000000000000000000 ) ) ;
#13334 = AXIS2_PLACEMENT_3D ( 'NONE', #10006, #5481, #8006 ) ;
#13335 = EDGE_LOOP ( 'NONE', ( #3507, #4498, #91, #10642 ) ) ;
#13336 = ORIENTED_EDGE ( 'NONE', *, *, #6469, .F. ) ;
#13337 = ORIENTED_EDGE ( 'NONE', *, *, #2797, .T. ) ;
#13338 = DIRECTION ( 'NONE',  ( 0.7071067811865516806, 8.659560562354882322E-17, 0.7071067811865433539 ) ) ;
#13339 = CARTESIAN_POINT ( 'NONE',  ( 3.875000000000000000, 3.137999999999999901, -0.5174999999999995159 ) ) ;
#13340 = CARTESIAN_POINT ( 'NONE',  ( 4.217173919807448712, 0.9311135807922138463, 0.3649311961389214987 ) ) ;
#13341 = AXIS2_PLACEMENT_3D ( 'NONE', #5640, #4483, #13487 ) ;
#13342 = DIRECTION ( 'NONE',  ( 0.000000000000000000, 0.000000000000000000, 1.000000000000000000 ) ) ;
#13343 = EDGE_LOOP ( 'NONE', ( #5500, #13601, #3689, #1894, #11909 ) ) ;
#13344 = LINE ( 'NONE', #412, #14841 ) ;
#13345 = DIRECTION ( 'NONE',  ( 0.000000000000000000, 0.000000000000000000, -1.000000000000000000 ) ) ;
#13346 = DIRECTION ( 'NONE',  ( -0.000000000000000000, 1.000000000000000000, -0.000000000000000000 ) ) ;
#13347 = TOROIDAL_SURFACE ( 'NONE', #8505, 1.409999999999999920, 0.05999999999999999778 ) ;
#13348 = EDGE_CURVE ( 'NONE', #11127, #11415, #9204, .T. ) ;
#13349 = DIRECTION ( 'NONE',  ( 0.000000000000000000, 0.000000000000000000, -1.000000000000000000 ) ) ;
#13350 = CARTESIAN_POINT ( 'NONE',  ( 0.000000000000000000, 1.000000000000000000, -1.000000000000000000 ) ) ;
#13351 = ADVANCED_FACE ( 'NONE', ( #3165 ), #11111, .F. ) ;
#13352 = CARTESIAN_POINT ( 'NONE',  ( 3.341229073668624316, 1.997163125837124076, 0.6280186637500814184 ) ) ;
#13354 = ORIENTED_EDGE ( 'NONE', *, *, #11010, .T. ) ;
#13353 = LINE ( 'NONE', #6274, #8902 ) ;
#13355 = AXIS2_PLACEMENT_3D ( 'NONE', #11065, #12285, #6484 ) ;
#13356 = EDGE_LOOP ( 'NONE', ( #13946, #4501, #878, #1889 ) ) ;
#13357 = CARTESIAN_POINT ( 'NONE',  ( -0.4150198198413779238, 1.581125151349165758, -0.04307009183866805646 ) ) ;
#13359 = ORIENTED_EDGE ( 'NONE', *, *, #6469, .T. ) ;
#13358 = DIRECTION ( 'NONE',  ( 1.000000000000000000, 0.000000000000000000, 0.000000000000000000 ) ) ;
#13360 = ORIENTED_EDGE ( 'NONE', *, *, #4647, .T. ) ;
#13361 = VECTOR ( 'NONE', #13150, 39.37007874015748143 ) ;
#13362 = CARTESIAN_POINT ( 'NONE',  ( 0.6583858180919160974, -0.06301918258053597344, 0.5137832783427485062 ) ) ;
#13363 = CARTESIAN_POINT ( 'NONE',  ( 0.000000000000000000, 0.000000000000000000, 0.000000000000000000 ) ) ;
#13364 = EDGE_LOOP ( 'NONE', ( #8826, #649, #6072, #403 ) ) ;
#13365 = DIRECTION ( 'NONE',  ( -1.000000000000000000, 0.000000000000000000, 0.000000000000000000 ) ) ;
#13366 = DIRECTION ( 'NONE',  ( -0.7070715176384831935, -0.7070715176384805289, 0.009986885842351455114 ) ) ;
#13367 = CARTESIAN_POINT ( 'NONE',  ( 0.6821548861276044429, -0.006955760605970391988, 0.4605830663053103735 ) ) ;
#13368 = CARTESIAN_POINT ( 'NONE',  ( 1.014923485655622848, -0.4429443392323548223, -0.3809436922965903083 ) ) ;
#13369 = CIRCLE ( 'NONE', #1380, 0.2812500000000000555 ) ;
#13370 = EDGE_CURVE ( 'NONE', #10812, #2681, #8064, .T. ) ;
#13371 = ORIENTED_EDGE ( 'NONE', *, *, #12218, .T. ) ;
#13372 = EDGE_CURVE ( 'NONE', #2396, #167, #830, .T. ) ;
#13373 = DIRECTION ( 'NONE',  ( 0.000000000000000000, 0.000000000000000000, -1.000000000000000000 ) ) ;
#13374 = DIRECTION ( 'NONE',  ( 0.000000000000000000, 0.000000000000000000, 1.000000000000000000 ) ) ;
#13375 = AXIS2_PLACEMENT_3D ( 'NONE', #8961, #1979, #10107 ) ;
#13376 = DIRECTION ( 'NONE',  ( 1.000000000000000000, 0.000000000000000000, 0.000000000000000000 ) ) ;
#13377 = ORIENTED_EDGE ( 'NONE', *, *, #9081, .F. ) ;
#13378 = CIRCLE ( 'NONE', #8766, 0.3750000000000004996 ) ;
#13379 = AXIS2_PLACEMENT_3D ( 'NONE', #1645, #6337, #9702 ) ;
#13380 = DIRECTION ( 'NONE',  ( -1.000000000000000000, -0.000000000000000000, -0.000000000000000000 ) ) ;
#13381 = CARTESIAN_POINT ( 'NONE',  ( 5.546318247523970513, 2.103182086337546510E-16, -1.502725933896874810 ) ) ;
#13382 = ORIENTED_EDGE ( 'NONE', *, *, #13602, .T. ) ;
#13383 = VECTOR ( 'NONE', #11942, 39.37007874015748143 ) ;
#13384 = CARTESIAN_POINT ( 'NONE',  ( 0.7023826192914041089, -0.05114289342557994111, 0.4896101277505872651 ) ) ;
#13385 = VERTEX_POINT ( 'NONE', #14932 ) ;
#13386 = CARTESIAN_POINT ( 'NONE',  ( 2.683697947871302336, 0.4122708231251094313, -0.4026504426247255464 ) ) ;
#13387 = AXIS2_PLACEMENT_3D ( 'NONE', #10424, #2467, #4690 ) ;
#13388 = CARTESIAN_POINT ( 'NONE',  ( 0.4108223460329304411, 4.529999999999999361, -0.2849999999999985323 ) ) ;
#13389 = VECTOR ( 'NONE', #12091, 39.37007874015748143 ) ;
#13390 = CARTESIAN_POINT ( 'NONE',  ( 1.503855556006640004, -0.3209522984523814904, 0.4787591023162903747 ) ) ;
#13391 = CARTESIAN_POINT ( 'NONE',  ( 0.8264521039527233937, -0.4832232234379731373, -0.3598827494686853701 ) ) ;
#13392 = VECTOR ( 'NONE', #2393, 39.37007874015748143 ) ;
#13393 = DIRECTION ( 'NONE',  ( 0.000000000000000000, 0.000000000000000000, 1.000000000000000000 ) ) ;
#13394 = AXIS2_PLACEMENT_3D ( 'NONE', #4191, #560, #9846 ) ;
#13395 = VECTOR ( 'NONE', #11831, 39.37007874015748143 ) ;
#13396 = DIRECTION ( 'NONE',  ( -1.000000000000000000, -0.000000000000000000, 0.000000000000000000 ) ) ;
#13397 = EDGE_CURVE ( 'NONE', #2101, #12746, #13784, .T. ) ;
#13398 = CARTESIAN_POINT ( 'NONE',  ( 1.775981552640435668, 0.05988294188168103577, -0.4749155147932142551 ) ) ;
#13399 = SURFACE_STYLE_USAGE ( .BOTH. , #14783 ) ;
#13400 = LINE ( 'NONE', #6535, #9622 ) ;
#13401 = ORIENTED_EDGE ( 'NONE', *, *, #2303, .F. ) ;
#13402 = ORIENTED_EDGE ( 'NONE', *, *, #4178, .T. ) ;
#13403 = ORIENTED_EDGE ( 'NONE', *, *, #13901, .T. ) ;
#13404 = CARTESIAN_POINT ( 'NONE',  ( 8.802840746862885979, 0.9385542876807506651, -0.1899546695978221456 ) ) ;
#13405 = ORIENTED_EDGE ( 'NONE', *, *, #5878, .T. ) ;
#13406=STYLED_ITEM('',(#15199),#10666);
#13407 = CARTESIAN_POINT ( 'NONE',  ( 2.774999999999999911, 1.272861240058668140E-16, -1.039370078740158965 ) ) ;
#13408 = LINE ( 'NONE', #6239, #14211 ) ;
#13409 = AXIS2_PLACEMENT_3D ( 'NONE', #1707, #11046, #5238 ) ;
#13410 = CARTESIAN_POINT ( 'NONE',  ( 4.386459485047407902, 1.780485827611695493, 0.5505562060287755299 ) ) ;
#13411 = EDGE_CURVE ( 'NONE', #5690, #1151, #833, .T. ) ;
#13412 = EDGE_CURVE ( 'NONE', #13039, #1808, #6970, .T. ) ;
#13413 = VERTEX_POINT ( 'NONE', #5531 ) ;
#13414 = EDGE_CURVE ( 'NONE', #5982, #7869, #11412, .T. ) ;
#13415 = LINE ( 'NONE', #6323, #7607 ) ;
#13416 = ORIENTED_EDGE ( 'NONE', *, *, #13320, .F. ) ;
#13417 = ORIENTED_EDGE ( 'NONE', *, *, #2964, .F. ) ;
#13418 = EDGE_CURVE ( 'NONE', #7097, #3105, #9894, .T. ) ;
#13419 = ORIENTED_EDGE ( 'NONE', *, *, #13093, .T. ) ;
#13420 = CARTESIAN_POINT ( 'NONE',  ( 0.000000000000000000, 0.000000000000000000, 0.000000000000000000 ) ) ;
#13421 = CARTESIAN_POINT ( 'NONE',  ( 0.000000000000000000, 0.000000000000000000, 0.000000000000000000 ) ) ;
#13422 = CARTESIAN_POINT ( 'NONE',  ( 4.322772591681486531, 0.9749115779099136736, 0.2230826791404775244 ) ) ;
#13423 = ITEM_DEFINED_TRANSFORMATION ( 'NONE', 'NONE', #4010,  #8424 ) ;
#13424 = FACE_OUTER_BOUND ( 'NONE', #5466, .T. ) ;
#13425 = EDGE_LOOP ( 'NONE', ( #15060, #13868, #8396, #1121 ) ) ;
#13426 = CYLINDRICAL_SURFACE ( 'NONE', #5322, 1.000000000000000222 ) ;
#13427 = PLANE ( 'NONE',  #7314 ) ;
#13428 = CARTESIAN_POINT ( 'NONE',  ( -0.3725000000000000533, 0.1859999999999983611, 0.3724999999999999423 ) ) ;
#13429 = EDGE_CURVE ( 'NONE', #11449, #436, #9123, .T. ) ;
#13430 = LINE ( 'NONE', #5343, #14057 ) ;
#13431 = DIRECTION ( 'NONE',  ( 0.000000000000000000, 0.000000000000000000, 1.000000000000000000 ) ) ;
#13432 = CARTESIAN_POINT ( 'NONE',  ( 3.426491571325181340, -3.360000000000000320, 0.9799999999999999822 ) ) ;
#13433 = CARTESIAN_POINT ( 'NONE',  ( 4.045956536581743812, 1.738919081015790846, 0.7773475529263453865 ) ) ;
#13435 = VERTEX_POINT ( 'NONE', #11872 ) ;
#13434 = DIRECTION ( 'NONE',  ( -1.000000000000000000, -0.000000000000000000, -0.000000000000000000 ) ) ;
#13436 = ORIENTED_EDGE ( 'NONE', *, *, #14550, .F. ) ;
#13437 = CARTESIAN_POINT ( 'NONE',  ( 3.874999999999999556, 3.137999999999999901, -1.130000000000000560 ) ) ;
#13438 = ORIENTED_EDGE ( 'NONE', *, *, #1769, .T. ) ;
#13439 = EDGE_LOOP ( 'NONE', ( #14475, #12354, #14047, #5399 ) ) ;
#13440 = EDGE_CURVE ( 'NONE', #7690, #5428, #9669, .T. ) ;
#13441 = PLANE ( 'NONE',  #9241 ) ;
#13442 = DIRECTION ( 'NONE',  ( -0.000000000000000000, -1.000000000000000000, -0.000000000000000000 ) ) ;
#13443 = ORIENTED_EDGE ( 'NONE', *, *, #3123, .T. ) ;
#13444 = DIRECTION ( 'NONE',  ( 0.000000000000000000, 0.000000000000000000, -1.000000000000000000 ) ) ;
#13445 = DIRECTION ( 'NONE',  ( 0.000000000000000000, -1.000000000000000000, 0.000000000000000000 ) ) ;
#13446 = ADVANCED_FACE ( 'NONE', ( #7294 ), #9358, .F. ) ;
#13447 = CARTESIAN_POINT ( 'NONE',  ( 0.000000000000000000, 1.559103846021539619, 0.000000000000000000 ) ) ;
#13448 = CIRCLE ( 'NONE', #5651, 0.4070000000000022489 ) ;
#13449 = CARTESIAN_POINT ( 'NONE',  ( 0.9699790962219284607, -0.4829911415283998921, -0.4026641122740337586 ) ) ;
#13450 = ORIENTED_EDGE ( 'NONE', *, *, #501, .T. ) ;
#13451 = CARTESIAN_POINT ( 'NONE',  ( 0.09500000000000431710, -1.679378605318048390, 1.679378605318054163 ) ) ;
#13452 = CARTESIAN_POINT ( 'NONE',  ( 3.426491571325181340, 1.987932976489903414, 0.2209981660730357955 ) ) ;
#13453 = FACE_OUTER_BOUND ( 'NONE', #186, .T. ) ;
#13454 = VERTEX_POINT ( 'NONE', #3766 ) ;
#13455 = CIRCLE ( 'NONE', #492, 0.1050000000000001071 ) ;
#13456 = CARTESIAN_POINT ( 'NONE',  ( 0.7513246802501660770, -0.4429999999999998939, 0.4293820849162031661 ) ) ;
#13457 = LINE ( 'NONE', #376, #9684 ) ;
#13458 = VERTEX_POINT ( 'NONE', #9288 ) ;
#13459 = DIRECTION ( 'NONE',  ( 0.000000000000000000, 0.000000000000000000, 1.000000000000000000 ) ) ;
#13460 = VERTEX_POINT ( 'NONE', #68 ) ;
#13461 = EDGE_CURVE ( 'NONE', #15105, #4070, #10502, .T. ) ;
#13462 = ADVANCED_FACE ( 'NONE', ( #6061, #6988, #1454 ), #143, .F. ) ;
#13463 = EDGE_CURVE ( 'NONE', #9247, #4088, #8450, .T. ) ;
#13464 = CARTESIAN_POINT ( 'NONE',  ( 3.874999999999999556, 3.137999999999999901, 1.320000000000000062 ) ) ;
#13465 = CARTESIAN_POINT ( 'NONE',  ( 0.8374688766003500762, -0.4832241325771656770, -0.3334326046303043856 ) ) ;
#13466 = CIRCLE ( 'NONE', #9087, 0.4850000000000000977 ) ;
#13467 = CARTESIAN_POINT ( 'NONE',  ( 0.9672649160634325671, -0.4430530727333169549, -0.4081727571047788494 ) ) ;
#13468 = ORIENTED_EDGE ( 'NONE', *, *, #10757, .T. ) ;
#13469 = LINE ( 'NONE', #998, #9668 ) ;
#13470 = DIRECTION ( 'NONE',  ( 0.000000000000000000, 0.000000000000000000, 1.000000000000000000 ) ) ;
#13471 = ORIENTED_EDGE ( 'NONE', *, *, #8075, .T. ) ;
#13472 = ORIENTED_EDGE ( 'NONE', *, *, #3537, .F. ) ;
#13473 = ORIENTED_EDGE ( 'NONE', *, *, #198, .T. ) ;
#13474 = LINE ( 'NONE', #3016, #11838 ) ;
#13475 = CARTESIAN_POINT ( 'NONE',  ( 0.6552631510457631592, -0.4102150000379021222, -0.5075199847260437602 ) ) ;
#13476 = EDGE_CURVE ( 'NONE', #13413, #5032, #9512, .T. ) ;
#13477 = PRODUCT_DEFINITION_SHAPE ( 'NONE', 'NONE',  #15163 ) ;
#13478 = EDGE_CURVE ( 'NONE', #184, #11754, #10390, .T. ) ;
#13479 = CARTESIAN_POINT ( 'NONE',  ( 0.3724999999999999423, -0.6290000000000003366, 0.4124999999999999223 ) ) ;
#13480 = DIRECTION ( 'NONE',  ( 0.000000000000000000, -1.000000000000000000, 0.000000000000000000 ) ) ;
#13481 = CARTESIAN_POINT ( 'NONE',  ( 2.372634528609597115, 0.1852128444980938871, 0.4664882128727457777 ) ) ;
#13482 = AXIS2_PLACEMENT_3D ( 'NONE', #10952, #1749, #8589 ) ;
#13483 = ORIENTED_EDGE ( 'NONE', *, *, #4824, .T. ) ;
#13484 = ORIENTED_EDGE ( 'NONE', *, *, #1277, .T. ) ;
#13485 = ORIENTED_EDGE ( 'NONE', *, *, #13612, .F. ) ;
#13486 = EDGE_LOOP ( 'NONE', ( #9212, #8369, #12258, #2226 ) ) ;
#13487 = DIRECTION ( 'NONE',  ( 0.000000000000000000, 0.000000000000000000, 1.000000000000000000 ) ) ;
#13488 = EDGE_CURVE ( 'NONE', #14644, #4727, #5499, .T. ) ;
#13489 = DIRECTION ( 'NONE',  ( -0.000000000000000000, -1.000000000000000000, -0.000000000000000000 ) ) ;
#13490 = FACE_OUTER_BOUND ( 'NONE', #8130, .T. ) ;
#13491 = ITEM_DEFINED_TRANSFORMATION ( 'NONE', 'NONE', #4505,  #8424 ) ;
#13492 = DIRECTION ( 'NONE',  ( 0.000000000000000000, 0.000000000000000000, 1.000000000000000000 ) ) ;
#13493 = ORIENTED_EDGE ( 'NONE', *, *, #11996, .T. ) ;
#13494 = FACE_OUTER_BOUND ( 'NONE', #10165, .T. ) ;
#13495 = CARTESIAN_POINT ( 'NONE',  ( 6.215861650065340527, 0.000000000000000000, 3.000000000000000444 ) ) ;
#13496 = CARTESIAN_POINT ( 'NONE',  ( 0.000000000000000000, 1.000000000000000000, 0.6614378277661475680 ) ) ;
#13497 = LINE ( 'NONE', #8932, #6139 ) ;
#13498 = AXIS2_PLACEMENT_3D ( 'NONE', #3472, #6000, #8231 ) ;
#13499 = CARTESIAN_POINT ( 'NONE',  ( 3.874999999999999556, 3.535499999999999421, -1.320000000000000062 ) ) ;
#13500 = CARTESIAN_POINT ( 'NONE',  ( -0.09035531712817639061, 1.629999999999999893, -0.1564999999999998892 ) ) ;
#13501 = CARTESIAN_POINT ( 'NONE',  ( 4.014119211518829111, 1.817012082641814574, 0.7380940613581021825 ) ) ;
#13503 = ORIENTED_EDGE ( 'NONE', *, *, #1938, .F. ) ;
#13502 = DIRECTION ( 'NONE',  ( -1.000000000000000000, -0.000000000000000000, -0.000000000000000000 ) ) ;
#13504 = ORIENTED_EDGE ( 'NONE', *, *, #6560, .F. ) ;
#13505 = VECTOR ( 'NONE', #4455, 39.37007874015748143 ) ;
#13507 = EDGE_LOOP ( 'NONE', ( #2376, #12494 ) ) ;
#13506 = FACE_OUTER_BOUND ( 'NONE', #2527, .T. ) ;
#13508 = ORIENTED_EDGE ( 'NONE', *, *, #3098, .F. ) ;
#13509 = EDGE_CURVE ( 'NONE', #1808, #11506, #5915, .T. ) ;
#13510 = AXIS2_PLACEMENT_3D ( 'NONE', #12908, #8187, #5659 ) ;
#13511 = EDGE_CURVE ( 'NONE', #13774, #2273, #2306, .T. ) ;
#13512 = CARTESIAN_POINT ( 'NONE',  ( 0.6678556410416569555, 0.02086291274669062334, 0.4666787114416893201 ) ) ;
#13513 = DIRECTION ( 'NONE',  ( 0.7071067811865496822, 8.659560562354905741E-17, 0.7071067811865452413 ) ) ;
#13514 = ORIENTED_EDGE ( 'NONE', *, *, #1136, .F. ) ;
#13515 = EDGE_CURVE ( 'NONE', #4759, #6131, #12812, .T. ) ;
#13516 = DIRECTION ( 'NONE',  ( 1.000000000000000000, 0.000000000000000000, 0.000000000000000000 ) ) ;
#13517 = DIRECTION ( 'NONE',  ( -1.000000000000000000, -0.000000000000000000, -0.000000000000000000 ) ) ;
#13518 = EDGE_CURVE ( 'NONE', #2188, #7512, #334, .T. ) ;
#13519 = CARTESIAN_POINT ( 'NONE',  ( -0.3725000000000000533, 0.1859999999999983611, 0.4124999999999999223 ) ) ;
#13520 = VECTOR ( 'NONE', #14912, 39.37007874015748143 ) ;
#13521 = LINE ( 'NONE', #3062, #11945 ) ;
#13522 = DIRECTION ( 'NONE',  ( 0.000000000000000000, 0.000000000000000000, 1.000000000000000000 ) ) ;
#13523 = ORIENTED_EDGE ( 'NONE', *, *, #11618, .T. ) ;
#13524 = CARTESIAN_POINT ( 'NONE',  ( 3.426491571325181340, -1.679378605318041950, 1.416878605318058870 ) ) ;
#13525 = CARTESIAN_POINT ( 'NONE',  ( 3.374989204712153246, 1.000005397643052074, 0.01633309950357363094 ) ) ;
#13526 = CARTESIAN_POINT ( 'NONE',  ( 4.040517861103548825, 1.740199758096359961, -0.7780251460681402165 ) ) ;
#13527 = VERTEX_POINT ( 'NONE', #1148 ) ;
#13528 = CARTESIAN_POINT ( 'NONE',  ( 3.891802077818124150, 0.8660254037844385966, -0.5000000000000002220 ) ) ;
#13529 = DIRECTION ( 'NONE',  ( 1.000000000000000000, 0.000000000000000000, 0.000000000000000000 ) ) ;
#13530 = ORIENTED_EDGE ( 'NONE', *, *, #6699, .F. ) ;
#13531 = AXIS2_PLACEMENT_3D ( 'NONE', #4052, #1670, #6362 ) ;
#13532 = CYLINDRICAL_SURFACE ( 'NONE', #14002, 0.05999999999999995615 ) ;
#13533 = ORIENTED_EDGE ( 'NONE', *, *, #4009, .F. ) ;
#13534 = FILL_AREA_STYLE_COLOUR ( '', #11469 ) ;
#13535 = VECTOR ( 'NONE', #13006, 39.37007874015748143 ) ;
#13536 = CARTESIAN_POINT ( 'NONE',  ( 3.599064736766494743, 1.969292692958134472, -0.6979109735870647757 ) ) ;
#13537 = EDGE_CURVE ( 'NONE', #15007, #2639, #3533, .T. ) ;
#13538 = FACE_OUTER_BOUND ( 'NONE', #7290, .T. ) ;
#13539 = CARTESIAN_POINT ( 'NONE',  ( 3.426491571325181340, 1.575000000000016609, 1.575000000000000178 ) ) ;
#13540 = DIRECTION ( 'NONE',  ( -1.000000000000000000, -0.000000000000000000, -0.000000000000000000 ) ) ;
#13541 = EDGE_CURVE ( 'NONE', #11167, #3810, #4689, .T. ) ;
#13542 = ORIENTED_EDGE ( 'NONE', *, *, #1029, .T. ) ;
#13543 = CARTESIAN_POINT ( 'NONE',  ( 3.875000000000000000, 3.567999999999999616, 0.000000000000000000 ) ) ;
#13544 = CARTESIAN_POINT ( 'NONE',  ( 0.8258105267240533065, -0.4829999999999998184, -0.3634189688144888741 ) ) ;
#13545 = CIRCLE ( 'NONE', #100, 0.1250000000000000278 ) ;
#13546 = AXIS2_PLACEMENT_3D ( 'NONE', #12938, #4612, #13923 ) ;
#13547 = EDGE_CURVE ( 'NONE', #5886, #10348, #14773, .T. ) ;
#13548 = FACE_OUTER_BOUND ( 'NONE', #12966, .T. ) ;
#13549 = ORIENTED_EDGE ( 'NONE', *, *, #4592, .F. ) ;
#13550 = VERTEX_POINT ( 'NONE', #9435 ) ;
#13551 = LINE ( 'NONE', #13853, #6760 ) ;
#13552 = EDGE_LOOP ( 'NONE', ( #279, #4709, #4085, #4171 ) ) ;
#13553 = DIRECTION ( 'NONE',  ( 0.000000000000000000, -9.641816448226552334E-15, -1.000000000000000000 ) ) ;
#13554 = CARTESIAN_POINT ( 'NONE',  ( 0.6766092641689801512, -0.4260904363423368424, -0.4729901586420192094 ) ) ;
#13555 = AXIS2_PLACEMENT_3D ( 'NONE', #6442, #594, #9881 ) ;
#13556 = LINE ( 'NONE', #1085, #12940 ) ;
#13557 = CONICAL_SURFACE ( 'NONE', #2338, 0.4070000000000022489, 0.7853981633974547183 ) ;
#13558 = AXIS2_PLACEMENT_3D ( 'NONE', #1059, #9112, #11556 ) ;
#13559 = CARTESIAN_POINT ( 'NONE',  ( 4.548733854531023191, 1.796245319939208107, -0.3336101870576589357 ) ) ;
#13560 = ORIENTED_EDGE ( 'NONE', *, *, #1412, .F. ) ;
#13561 = EDGE_CURVE ( 'NONE', #4391, #3525, #14081, .T. ) ;
#13562 = AXIS2_PLACEMENT_3D ( 'NONE', #14767, #3155, #2138 ) ;
#13563 = EDGE_LOOP ( 'NONE', ( #2154, #8792 ) ) ;
#13564 = AXIS2_PLACEMENT_3D ( 'NONE', #13207, #2744, #14214 ) ;
#13565 = ORIENTED_EDGE ( 'NONE', *, *, #3436, .F. ) ;
#13566 = AXIS2_PLACEMENT_3D ( 'NONE', #14108, #2566, #6015 ) ;
#13567 = ORIENTED_EDGE ( 'NONE', *, *, #10775, .T. ) ;
#13568 = DIRECTION ( 'NONE',  ( -0.000000000000000000, 1.000000000000000000, -0.000000000000000000 ) ) ;
#13569 = DIRECTION ( 'NONE',  ( 1.000000000000000000, -0.000000000000000000, -0.000000000000000000 ) ) ;
#13570 = CARTESIAN_POINT ( 'NONE',  ( 1.250000000000000222, -0.05999999999999997696, -0.4823446327683615364 ) ) ;
#13571 = ITEM_DEFINED_TRANSFORMATION ( 'NONE', 'NONE', #11331,  #8424 ) ;
#13572 = CARTESIAN_POINT ( 'NONE',  ( 2.124999999999999556, 2.360000000000000320, -0.9800000000000007594 ) ) ;
#13573 = EDGE_LOOP ( 'NONE', ( #1944, #7335, #9811, #6220 ) ) ;
#13574 = CARTESIAN_POINT ( 'NONE',  ( 2.774999999999999911, 0.7000000000000030642, 2.399999999999999911 ) ) ;
#13575 = CARTESIAN_POINT ( 'NONE',  ( 0.4193347797797013499, 0.000000000000000000, -1.564978703518711711 ) ) ;
#13576 = VECTOR ( 'NONE', #8183, 39.37007874015748854 ) ;
#13577 = FACE_OUTER_BOUND ( 'NONE', #3467, .T. ) ;
#13578 = DIRECTION ( 'NONE',  ( 0.9743309173630048114, 0.2251205531944285021, 0.000000000000000000 ) ) ;
#13579 = DIRECTION ( 'NONE',  ( 0.000000000000000000, 0.000000000000000000, 1.000000000000000000 ) ) ;
#13580 = DIRECTION ( 'NONE',  ( 0.3420201433256623846, 0.000000000000000000, -0.9396926207859106484 ) ) ;
#13581 = ADVANCED_FACE ( 'NONE', ( #2466 ), #1297, .F. ) ;
#13582 = CARTESIAN_POINT ( 'NONE',  ( 4.454384321854326423, 1.730788856496732420, 0.4784941975638398737 ) ) ;
#13584 = ORIENTED_EDGE ( 'NONE', *, *, #5785, .F. ) ;
#13583 = CARTESIAN_POINT ( 'NONE',  ( 3.621412531120375089, 1.971946916245812975, -0.4310735882759350046 ) ) ;
#13585 = AXIS2_PLACEMENT_3D ( 'NONE', #6334, #9838, #14491 ) ;
#13586 = VERTEX_POINT ( 'NONE', #7503 ) ;
#13588 = ORIENTED_EDGE ( 'NONE', *, *, #3461, .T. ) ;
#13587 = CARTESIAN_POINT ( 'NONE',  ( 0.8999999999999998002, 0.1749999999999999889, -0.2749999999999993006 ) ) ;
#13589 = ORIENTED_EDGE ( 'NONE', *, *, #6344, .T. ) ;
#13590 = PLANE ( 'NONE',  #2401 ) ;
#13591 = DIRECTION ( 'NONE',  ( 1.000000000000000000, 0.000000000000000000, -3.779312718515659280E-16 ) ) ;
#13592 = VERTEX_POINT ( 'NONE', #1528 ) ;
#13593 = AXIS2_PLACEMENT_3D ( 'NONE', #10225, #9007, #9079 ) ;
#13594 = CARTESIAN_POINT ( 'NONE',  ( -0.2100000000000000200, 1.559103846021539619, -0.3809527529760087239 ) ) ;
#13595 = CYLINDRICAL_SURFACE ( 'NONE', #4608, 1.124999999999999778 ) ;
#13596 = AXIS2_PLACEMENT_3D ( 'NONE', #1554, #2791, #7246 ) ;
#13597 = DIRECTION ( 'NONE',  ( 0.8682164115033647045, 0.000000000000000000, -0.4961857140186728410 ) ) ;
#13598 = ADVANCED_FACE ( 'NONE', ( #5282 ), #10395, .F. ) ;
#13599 = CARTESIAN_POINT ( 'NONE',  ( 1.012991562538327006, -0.4429593234937804214, -0.3529545607104379590 ) ) ;
#13600 = EDGE_CURVE ( 'NONE', #10755, #13592, #585, .T. ) ;
#13601 = ORIENTED_EDGE ( 'NONE', *, *, #8401, .T. ) ;
#13602 = EDGE_CURVE ( 'NONE', #12982, #2178, #1744, .T. ) ;
#13603 = FACE_OUTER_BOUND ( 'NONE', #5933, .T. ) ;
#13604 = CARTESIAN_POINT ( 'NONE',  ( 3.569652111961249652, 0.9182054424553791616, -0.3962596773958052543 ) ) ;
#13605 = CIRCLE ( 'NONE', #401, 0.9999999999999998890 ) ;
#13606 = LINE ( 'NONE', #13831, #3779 ) ;
#13607 = ORIENTED_EDGE ( 'NONE', *, *, #14689, .F. ) ;
#13608 = PRODUCT_DEFINITION_SHAPE ( 'NONE', 'NONE',  #15154 ) ;
#13609 = CARTESIAN_POINT ( 'NONE',  ( 4.280825855804681446, 0.9563621563813751170, -0.2925165865892054851 ) ) ;
#13610 = DIRECTION ( 'NONE',  ( -1.000000000000000000, 0.000000000000000000, -0.000000000000000000 ) ) ;
#13611 = ORIENTED_EDGE ( 'NONE', *, *, #2110, .T. ) ;
#13612 = EDGE_CURVE ( 'NONE', #7174, #8323, #7648, .T. ) ;
#13613 = FACE_OUTER_BOUND ( 'NONE', #11072, .T. ) ;
#13614 = ORIENTED_EDGE ( 'NONE', *, *, #12315, .T. ) ;
#13615 = PRESENTATION_STYLE_ASSIGNMENT (( #8972 ) ) ;
#13616 = VECTOR ( 'NONE', #1164, 39.37007874015748143 ) ;
#13617 = CARTESIAN_POINT ( 'NONE',  ( 2.684185600477509315, 0.4127059874557739705, -0.4620877740047383275 ) ) ;
#13618 = CARTESIAN_POINT ( 'NONE',  ( 3.835129291132573837, 1.869265298754045679, -0.7500000000000001110 ) ) ;
#13619 = AXIS2_PLACEMENT_3D ( 'NONE', #5357, #8577, #14515 ) ;
#13620 = CARTESIAN_POINT ( 'NONE',  ( 6.096491571325181269, 0.000000000000000000, 0.000000000000000000 ) ) ;
#13621 = CARTESIAN_POINT ( 'NONE',  ( 2.774999999999999911, -1.679378605318059048, -1.416878605318056872 ) ) ;
#13622 = DIRECTION ( 'NONE',  ( -1.000000000000000000, -1.365923996832131609E-16, 0.000000000000000000 ) ) ;
#13623 = VERTEX_POINT ( 'NONE', #12308 ) ;
#13624 = CIRCLE ( 'NONE', #9736, 0.05999999999999994227 ) ;
#13625 = DIRECTION ( 'NONE',  ( 0.000000000000000000, 0.000000000000000000, -1.000000000000000000 ) ) ;
#13626 = CARTESIAN_POINT ( 'NONE',  ( 3.874999999999999556, 2.750000000000000000, 1.097999999999997867 ) ) ;
#13627 = VECTOR ( 'NONE', #13366, 39.37007874015748143 ) ;
#13628 = DIRECTION ( 'NONE',  ( 0.7071067811865512365, 0.000000000000000000, -0.7071067811865436870 ) ) ;
#13629 = VERTEX_POINT ( 'NONE', #3214 ) ;
#13630 = ORIENTED_EDGE ( 'NONE', *, *, #3102, .F. ) ;
#13631 = DIRECTION ( 'NONE',  ( 0.000000000000000000, 0.000000000000000000, 1.000000000000000000 ) ) ;
#13632 = ORIENTED_EDGE ( 'NONE', *, *, #11510, .F. ) ;
#13633 = CARTESIAN_POINT ( 'NONE',  ( 3.426491571325181340, 2.359999999999994547, -1.575000000000016831 ) ) ;
#13634 = AXIS2_PLACEMENT_3D ( 'NONE', #14856, #13540, #14631 ) ;
#13635 = VECTOR ( 'NONE', #819, 39.37007874015748854 ) ;
#13636 = EDGE_CURVE ( 'NONE', #1866, #259, #2062, .T. ) ;
#13637 = FACE_OUTER_BOUND ( 'NONE', #4369, .T. ) ;
#13638 = AXIS2_PLACEMENT_3D ( 'NONE', #7223, #3466, #4 ) ;
#13639 = LINE ( 'NONE', #11583, #13884 ) ;
#13640 = CIRCLE ( 'NONE', #3884, 0.2499999999999999167 ) ;
#13641 = EDGE_CURVE ( 'NONE', #5162, #4450, #11352, .T. ) ;
#13642 = VECTOR ( 'NONE', #3799, 39.37007874015748143 ) ;
#13643 = CARTESIAN_POINT ( 'NONE',  ( 3.923683937046483550, 1.841036866441990050, -0.7489011557682658804 ) ) ;
#13644 = ORIENTED_EDGE ( 'NONE', *, *, #499, .T. ) ;
#13645 = VECTOR ( 'NONE', #515, 39.37007874015748143 ) ;
#13646 = VECTOR ( 'NONE', #5561, 39.37007874015748143 ) ;
#13647 = ORIENTED_EDGE ( 'NONE', *, *, #1257, .F. ) ;
#13648 = ORIENTED_EDGE ( 'NONE', *, *, #3515, .T. ) ;
#13649 = VECTOR ( 'NONE', #14720, 39.37007874015748143 ) ;
#13650 = UNCERTAINTY_MEASURE_WITH_UNIT (LENGTH_MEASURE( 1.000000000000000082E-05 ), #9552, 'distance_accuracy_value', 'NONE');
#13651 = ORIENTED_EDGE ( 'NONE', *, *, #2064, .F. ) ;
#13652 = LINE ( 'NONE', #9078, #7274 ) ;
#13653 = LINE ( 'NONE', #3028, #2378 ) ;
#13654 = CARTESIAN_POINT ( 'NONE',  ( 0.8999999999999998002, 0.1749999999999999889, -0.3799999999999999489 ) ) ;
#13655 = CONTEXT_DEPENDENT_SHAPE_REPRESENTATION ( #14077, #2992 ) ;
#13656 = CARTESIAN_POINT ( 'NONE',  ( -0.4108223460329323840, 5.750000000000000000, 0.2849999999999956457 ) ) ;
#13657 = VERTEX_POINT ( 'NONE', #7877 ) ;
#13658 = DIRECTION ( 'NONE',  ( -1.000000000000000000, -0.000000000000000000, -0.000000000000000000 ) ) ;
#13659 = ADVANCED_FACE ( 'NONE', ( #12527 ), #9357, .T. ) ;
#13660 = EDGE_CURVE ( 'NONE', #3117, #10543, #6658, .T. ) ;
#13661 = CARTESIAN_POINT ( 'NONE',  ( 0.6601485485260574215, -0.07064835164835239767, -0.5137583810202325241 ) ) ;
#13662 = VECTOR ( 'NONE', #5898, 39.37007874015748854 ) ;
#13663 = DIRECTION ( 'NONE',  ( -0.000000000000000000, -0.000000000000000000, 1.000000000000000000 ) ) ;
#13664 = CARTESIAN_POINT ( 'NONE',  ( 4.454242182452238907, 1.708366068422199957, 0.5527474542283296044 ) ) ;
#13665 = CARTESIAN_POINT ( 'NONE',  ( 6.826491571325181695, 0.000000000000000000, 0.000000000000000000 ) ) ;
#13667 = ORIENTED_EDGE ( 'NONE', *, *, #15000, .T. ) ;
#13666 = CARTESIAN_POINT ( 'NONE',  ( 3.874999999999999556, 3.567999999999999616, -1.320000000000000062 ) ) ;
#13668 = VERTEX_POINT ( 'NONE', #2129 ) ;
#13670 = VERTEX_POINT ( 'NONE', #814 ) ;
#13669 = DIRECTION ( 'NONE',  ( 1.000000000000000000, 0.000000000000000000, 0.000000000000000000 ) ) ;
#13671 = ORIENTED_EDGE ( 'NONE', *, *, #10945, .T. ) ;
#13672 = CIRCLE ( 'NONE', #14414, 0.2624999999999997335 ) ;
#13673 = CARTESIAN_POINT ( 'NONE',  ( 2.124999999999999556, -1.575000000000027489, -2.359999999999989218 ) ) ;
#13674 = CARTESIAN_POINT ( 'NONE',  ( -0.09035531712817639061, 1.379999999999999671, 0.1565000000000000280 ) ) ;
#13675 = ORIENTED_EDGE ( 'NONE', *, *, #1856, .F. ) ;
#13676 = DIRECTION ( 'NONE',  ( 0.000000000000000000, 0.000000000000000000, 1.000000000000000000 ) ) ;
#13677 = DIRECTION ( 'NONE',  ( 0.000000000000000000, 0.000000000000000000, 1.000000000000000000 ) ) ;
#13678 = FACE_OUTER_BOUND ( 'NONE', #10167, .T. ) ;
#13679 = CARTESIAN_POINT ( 'NONE',  ( 3.602264755523620465, 1.056999999999999940, -0.4491205543005138412 ) ) ;
#13680 = CARTESIAN_POINT ( 'NONE',  ( 0.9738485687486472253, -0.4432125501547143909, -0.3605661772192202408 ) ) ;
#13681 = ORIENTED_EDGE ( 'NONE', *, *, #6771, .T. ) ;
#13682 = DIRECTION ( 'NONE',  ( -1.224646799147354933E-16, 0.000000000000000000, -1.000000000000000000 ) ) ;
#13683 = CARTESIAN_POINT ( 'NONE',  ( 1.375000000000000000, 0.000000000000000000, 1.350000000000000089 ) ) ;
#13684 = LINE ( 'NONE', #5373, #11339 ) ;
#13685 = FACE_OUTER_BOUND ( 'NONE', #11327, .T. ) ;
#13687 = VERTEX_POINT ( 'NONE', #5512 ) ;
#13686 = FACE_OUTER_BOUND ( 'NONE', #9667, .T. ) ;
#13688 = VERTEX_POINT ( 'NONE', #6821 ) ;
#13689 = CARTESIAN_POINT ( 'NONE',  ( 0.9749999999999999778, -0.4829448521957645513, -0.3750000000000000555 ) ) ;
#13690 = ORIENTED_EDGE ( 'NONE', *, *, #12016, .F. ) ;
#13691 = COLOUR_RGB ( '',0.7921568627450980005, 0.8196078431372548767, 0.9333333333333333481 ) ;
#13692 = ADVANCED_FACE ( 'NONE', ( #11475 ), #11165, .F. ) ;
#13693 = SURFACE_STYLE_FILL_AREA ( #11104 ) ;
#13694 = CARTESIAN_POINT ( 'NONE',  ( 0.000000000000000000, 0.03800000000000004763, -0.1900000000000000577 ) ) ;
#13695 = DIRECTION ( 'NONE',  ( -0.000000000000000000, -1.000000000000000000, -0.000000000000000000 ) ) ;
#13696 = DIRECTION ( 'NONE',  ( 0.000000000000000000, 1.000000000000000000, 0.000000000000000000 ) ) ;
#13697 = EDGE_LOOP ( 'NONE', ( #6481, #10898 ) ) ;
#13698 = EDGE_CURVE ( 'NONE', #8959, #2536, #12384, .T. ) ;
#13699 = CARTESIAN_POINT ( 'NONE',  ( 0.5816197779170538817, 0.1749999999999999889, -1.650520655410200099 ) ) ;
#13700 = DIRECTION ( 'NONE',  ( 0.000000000000000000, 0.000000000000000000, -1.000000000000000000 ) ) ;
#13701 = CARTESIAN_POINT ( 'NONE',  ( 8.849999999999999645, 0.8820000000000000062, 0.5000000000000000000 ) ) ;
#13702 = VERTEX_POINT ( 'NONE', #4187 ) ;
#13703 = ORIENTED_EDGE ( 'NONE', *, *, #13245, .F. ) ;
#13704 = CARTESIAN_POINT ( 'NONE',  ( 2.124999999999999556, 1.679378605318059048, 1.679378605318041506 ) ) ;
#13705 = ORIENTED_EDGE ( 'NONE', *, *, #7277, .T. ) ;
#13706 = CARTESIAN_POINT ( 'NONE',  ( 0.000000000000000000, 3.673940397442060361E-16, -3.000000000000000444 ) ) ;
#13707 = ADVANCED_FACE ( 'NONE', ( #8777 ), #1569, .F. ) ;
#13708 = DIRECTION ( 'NONE',  ( -0.000000000000000000, -1.000000000000000000, -0.000000000000000000 ) ) ;
#13709 = EDGE_CURVE ( 'NONE', #8247, #628, #12086, .T. ) ;
#13710 = AXIS2_PLACEMENT_3D ( 'NONE', #10157, #4343, #6875 ) ;
#13711 = CARTESIAN_POINT ( 'NONE',  ( 3.874999999999999556, 3.170500000000000096, 1.130000000000000560 ) ) ;
#13712 = CARTESIAN_POINT ( 'NONE',  ( 0.000000000000000000, 1.603403463250997918, -0.3809527529760087239 ) ) ;
#13713 = ADVANCED_FACE ( 'NONE', ( #12280 ), #6336, .F. ) ;
#13714 = ORIENTED_EDGE ( 'NONE', *, *, #700, .F. ) ;
#13715 = ADVANCED_FACE ( 'NONE', ( #13490 ), #11871, .F. ) ;
#13716 = CARTESIAN_POINT ( 'NONE',  ( 3.669841109856190275, 1.848025286936557654, -0.7790857044152560418 ) ) ;
#13717 = ORIENTED_EDGE ( 'NONE', *, *, #4183, .F. ) ;
#13718 = ORIENTED_EDGE ( 'NONE', *, *, #3667, .T. ) ;
#13719 = CARTESIAN_POINT ( 'NONE',  ( 8.469665986256828205, 0.9969999999999998863, 6.829619984160658046E-17 ) ) ;
#13720 = EDGE_LOOP ( 'NONE', ( #11540, #12522 ) ) ;
#13721 = FACE_OUTER_BOUND ( 'NONE', #1291, .T. ) ;
#13722 = CARTESIAN_POINT ( 'NONE',  ( 0.000000000000000000, 0.000000000000000000, 0.000000000000000000 ) ) ;
#13723 = CARTESIAN_POINT ( 'NONE',  ( 0.8108060929038570785, -0.4429999999999998939, -0.3024090436974096185 ) ) ;
#13724 = CARTESIAN_POINT ( 'NONE',  ( 0.7513246802501660770, 0.05999999999999999778, 0.4293820849162031661 ) ) ;
#13725 = ORIENTED_EDGE ( 'NONE', *, *, #1820, .T. ) ;
#13726 = DIRECTION ( 'NONE',  ( -0.000000000000000000, -1.000000000000000000, -0.000000000000000000 ) ) ;
#13727 = CONICAL_SURFACE ( 'NONE', #6173, 0.2945000000000009277, 0.7853981633974503884 ) ;
#13728 = CARTESIAN_POINT ( 'NONE',  ( 0.7017867892446606470, 0.04143956043956046470, -0.4010711782184316343 ) ) ;
#13729 = CARTESIAN_POINT ( 'NONE',  ( 8.792093969802149189, 0.8799778768672790186, -0.1855527009831952900 ) ) ;
#13730 = ADVANCED_FACE ( 'NONE', ( #5250 ), #8214, .F. ) ;
#13731 = DIRECTION ( 'NONE',  ( -1.365923996832131609E-16, 1.000000000000000000, 0.000000000000000000 ) ) ;
#13732 = CARTESIAN_POINT ( 'NONE',  ( 4.266066090114608578, 1.710594575876754231, 0.6935905660327770228 ) ) ;
#13734 = ORIENTED_EDGE ( 'NONE', *, *, #13418, .T. ) ;
#13733 = CARTESIAN_POINT ( 'NONE',  ( 3.662127683554703417, 1.955924818698876244, -0.4525689758964896448 ) ) ;
#13735 = ADVANCED_FACE ( 'NONE', ( #13266 ), #1716, .F. ) ;
#13736 = ORIENTED_EDGE ( 'NONE', *, *, #1262, .T. ) ;
#13738 = VERTEX_POINT ( 'NONE', #5179 ) ;
#13737 = DIRECTION ( 'NONE',  ( -1.000000000000000000, -1.365923996832131609E-16, 0.000000000000000000 ) ) ;
#13739 = VERTEX_POINT ( 'NONE', #484 ) ;
#13740 = FACE_OUTER_BOUND ( 'NONE', #1608, .T. ) ;
#13741 = DIRECTION ( 'NONE',  ( -2.760291306546953049E-17, -0.3090836082398114026, -0.9510348695591864798 ) ) ;
#13742 = DIRECTION ( 'NONE',  ( -1.000000000000000000, -0.000000000000000000, -0.000000000000000000 ) ) ;
#13743 = ORIENTED_EDGE ( 'NONE', *, *, #2880, .F. ) ;
#13744 = DIRECTION ( 'NONE',  ( -1.000000000000000000, -0.000000000000000000, -0.000000000000000000 ) ) ;
#13745 = CARTESIAN_POINT ( 'NONE',  ( 0.6570999327328049811, -0.3875696543617488388, -0.5130307608016103638 ) ) ;
#13746 = CARTESIAN_POINT ( 'NONE',  ( 1.532626322880889402, 0.1749999999999999889, -0.5400755080658653506 ) ) ;
#13747 = CARTESIAN_POINT ( 'NONE',  ( 3.339621231359971798, 1.044107824239214777, -0.3927132934523872576 ) ) ;
#13748 = DIRECTION ( 'NONE',  ( 1.000000000000000000, 0.000000000000000000, 0.000000000000000000 ) ) ;
#13749 = ORIENTED_EDGE ( 'NONE', *, *, #3931, .T. ) ;
#13750 = PLANE ( 'NONE',  #6315 ) ;
#13751 = CONICAL_SURFACE ( 'NONE', #8893, 2.967999999999998639, 0.7853981633974482790 ) ;
#13752 = DIRECTION ( 'NONE',  ( 0.000000000000000000, 0.000000000000000000, 1.000000000000000000 ) ) ;
#13753 = LINE ( 'NONE', #8964, #11330 ) ;
#13754 = EDGE_CURVE ( 'NONE', #12377, #3810, #645, .T. ) ;
#13755 = DIRECTION ( 'NONE',  ( 0.000000000000000000, 0.000000000000000000, -1.000000000000000000 ) ) ;
#13757 = ORIENTED_EDGE ( 'NONE', *, *, #7995, .T. ) ;
#13756 = CARTESIAN_POINT ( 'NONE',  ( 6.176491571325181340, 1.679378605318059492, 1.272378605318039257 ) ) ;
#13758 = ORIENTED_EDGE ( 'NONE', *, *, #15034, .T. ) ;
#13759 = DIRECTION ( 'NONE',  ( 0.000000000000000000, 0.000000000000000000, -1.000000000000000000 ) ) ;
#13760 = ORIENTED_EDGE ( 'NONE', *, *, #1876, .F. ) ;
#13761 = DIRECTION ( 'NONE',  ( 0.000000000000000000, 0.000000000000000000, -1.000000000000000000 ) ) ;
#13762 = DIRECTION ( 'NONE',  ( 0.000000000000000000, 0.000000000000000000, -1.000000000000000000 ) ) ;
#13763 = CIRCLE ( 'NONE', #9145, 0.05999999999999997696 ) ;
#13764 = DIRECTION ( 'NONE',  ( 0.9659258262890698665, 0.000000000000000000, -0.2588190451025147443 ) ) ;
#13765 = DIRECTION ( 'NONE',  ( 0.000000000000000000, 0.000000000000000000, -1.000000000000000000 ) ) ;
#13766 = DIRECTION ( 'NONE',  ( -1.000000000000000000, -0.000000000000000000, -0.000000000000000000 ) ) ;
#13767 = ORIENTED_EDGE ( 'NONE', *, *, #28, .F. ) ;
#13768 = CARTESIAN_POINT ( 'NONE',  ( 1.000847373107698779, -0.3829999999999998961, 0.4858637376679703634 ) ) ;
#13769 = LINE ( 'NONE', #1848, #54 ) ;
#13770 = VERTEX_POINT ( 'NONE', #9042 ) ;
#13771 = VECTOR ( 'NONE', #14683, 39.37007874015748143 ) ;
#13772 = PRODUCT_DEFINITION ( 'UNKNOWN', '', #817, #12569 ) ;
#13773 = CARTESIAN_POINT ( 'NONE',  ( 4.769268701363833074, 3.137999999999999901, -0.3249191361593796734 ) ) ;
#13774 = VERTEX_POINT ( 'NONE', #4377 ) ;
#13775 = DIRECTION ( 'NONE',  ( -1.000000000000000000, 0.000000000000000000, 0.000000000000000000 ) ) ;
#13776 = CARTESIAN_POINT ( 'NONE',  ( 0.7849999999999999201, -0.4429999999999998939, -0.3750000000000000555 ) ) ;
#13777 = ORIENTED_EDGE ( 'NONE', *, *, #5294, .T. ) ;
#13778 = CARTESIAN_POINT ( 'NONE',  ( 2.889807021265108578, 0.6241886699583397702, 0.4591835166487979181 ) ) ;
#13779 = CARTESIAN_POINT ( 'NONE',  ( 0.7145271609291456993, -0.4320022011844609211, -0.4647412378891554452 ) ) ;
#13780 = CARTESIAN_POINT ( 'NONE',  ( 3.906623289280057325E-17, 1.249999999999999778, 0.3190000000000000058 ) ) ;
#13781 = AXIS2_PLACEMENT_3D ( 'NONE', #7266, #14205, #44 ) ;
#13782 = CARTESIAN_POINT ( 'NONE',  ( 2.124999999999999556, 1.679378605318042395, -1.973878605318058588 ) ) ;
#13783 = AXIS2_PLACEMENT_3D ( 'NONE', #5158, #13396, #9680 ) ;
#13784 = CIRCLE ( 'NONE', #6985, 0.4349999999999999978 ) ;
#13785 = CARTESIAN_POINT ( 'NONE',  ( 2.156999999999999140, -1.679378605318041950, 1.679378605318059048 ) ) ;
#13786 = ADVANCED_FACE ( 'NONE', ( #10190 ), #8936, .F. ) ;
#13787 = EDGE_CURVE ( 'NONE', #10523, #10316, #1753, .T. ) ;
#13788 = EDGE_CURVE ( 'NONE', #13228, #7297, #2818, .T. ) ;
#13789 = CARTESIAN_POINT ( 'NONE',  ( 3.880536119609262258, 1.799609107823162413, -0.7503340787926818800 ) ) ;
#13790 = ORIENTED_EDGE ( 'NONE', *, *, #1007, .F. ) ;
#13791 = ORIENTED_EDGE ( 'NONE', *, *, #14737, .F. ) ;
#13792 = AXIS2_PLACEMENT_3D ( 'NONE', #5692, #8987, #10349 ) ;
#13793 = CARTESIAN_POINT ( 'NONE',  ( 0.000000000000000000, 1.866025403784438819, -0.4999999999999995004 ) ) ;
#13794 = ORIENTED_EDGE ( 'NONE', *, *, #11377, .F. ) ;
#13795 = CARTESIAN_POINT ( 'NONE',  ( -0.3725000000000000533, 0.2159999999999999698, 0.3724999999999999423 ) ) ;
#13796 = AXIS2_PLACEMENT_3D ( 'NONE', #4212, #13516, #11082 ) ;
#13797 = VECTOR ( 'NONE', #4153, 39.37007874015748854 ) ;
#13798 = CARTESIAN_POINT ( 'NONE',  ( 0.6577550957999014347, -0.05999999999999997696, 0.4907096737881370130 ) ) ;
#13799 = DIRECTION ( 'NONE',  ( 1.000000000000000000, 0.000000000000000000, 0.000000000000000000 ) ) ;
#13800 = EDGE_CURVE ( 'NONE', #8150, #937, #6441, .T. ) ;
#13801 = CARTESIAN_POINT ( 'NONE',  ( -0.4125000000000001998, -0.6590000000000000302, -0.4125000000000000333 ) ) ;
#13802 = ORIENTED_EDGE ( 'NONE', *, *, #4878, .T. ) ;
#13803 = CARTESIAN_POINT ( 'NONE',  ( 3.126948208750839342, 2.499883650940541102, -0.02820439714893648725 ) ) ;
#13804 = CARTESIAN_POINT ( 'NONE',  ( 0.6733128806866804927, 0.02908293500952287974, -0.4545362700951161017 ) ) ;
#13805 = CONICAL_SURFACE ( 'NONE', #11876, 0.3750000000000007772, 0.7853981633974557175 ) ;
#13806 = CARTESIAN_POINT ( 'NONE',  ( 3.875000000000000000, 0.7099999999999984102, 0.000000000000000000 ) ) ;
#13807 = AXIS2_PLACEMENT_3D ( 'NONE', #8386, #2251, #5931 ) ;
#13808 = CONICAL_SURFACE ( 'NONE', #11641, 3.000000000000000444, 0.7853981633974415066 ) ;
#13809 = DIRECTION ( 'NONE',  ( 0.000000000000000000, 0.000000000000000000, -1.000000000000000000 ) ) ;
#13810 = CARTESIAN_POINT ( 'NONE',  ( 4.525792272712025444, 1.792887553598168759, -0.3759268146155863577 ) ) ;
#13812 = ORIENTED_EDGE ( 'NONE', *, *, #8764, .F. ) ;
#13811 = DIRECTION ( 'NONE',  ( 0.000000000000000000, 0.000000000000000000, 1.000000000000000000 ) ) ;
#13813 = VERTEX_POINT ( 'NONE', #3154 ) ;
#13815 = EDGE_LOOP ( 'NONE', ( #7631, #5037, #3251, #14238 ) ) ;
#13814 = DIRECTION ( 'NONE',  ( -1.000000000000000000, -0.000000000000000000, -0.000000000000000000 ) ) ;
#13816 = ORIENTED_EDGE ( 'NONE', *, *, #5124, .T. ) ;
#13817 = FACE_BOUND ( 'NONE', #13720, .T. ) ;
#13818 = VECTOR ( 'NONE', #5953, 39.37007874015748854 ) ;
#13819 = DIRECTION ( 'NONE',  ( 1.000000000000000000, 0.000000000000000000, 0.000000000000000000 ) ) ;
#13820 = EDGE_LOOP ( 'NONE', ( #5905, #14510 ) ) ;
#13821 = DIRECTION ( 'NONE',  ( -1.000000000000000000, 0.000000000000000000, 0.000000000000000000 ) ) ;
#13822 = CARTESIAN_POINT ( 'NONE',  ( 0.6583858180919160974, -0.3799808174194639343, -0.5137832783427485062 ) ) ;
#13823 = ADVANCED_FACE ( 'NONE', ( #13685 ), #7815, .F. ) ;
#13824 = CYLINDRICAL_SURFACE ( 'NONE', #12790, 2.000000000000000000 ) ;
#13825 = DIRECTION ( 'NONE',  ( 1.047444401652940007E-14, 0.000000000000000000, -1.000000000000000000 ) ) ;
#13826 = EDGE_CURVE ( 'NONE', #13163, #4070, #1984, .T. ) ;
#13827 = DIRECTION ( 'NONE',  ( -1.000000000000000000, 0.000000000000000000, -0.000000000000000000 ) ) ;
#13828 = DIRECTION ( 'NONE',  ( 0.000000000000000000, 1.000000000000000000, 0.000000000000000000 ) ) ;
#13829 = CARTESIAN_POINT ( 'NONE',  ( 2.124999999999999556, -1.679378605318059048, -1.973878605318026613 ) ) ;
#13830 = CARTESIAN_POINT ( 'NONE',  ( 7.623651669702752511E-17, -0.6589999999999998082, 0.000000000000000000 ) ) ;
#13831 = CARTESIAN_POINT ( 'NONE',  ( 0.8999999999999998002, 0.1749999999999999889, -0.4650000000000000244 ) ) ;
#13832 = DIRECTION ( 'NONE',  ( 0.000000000000000000, 0.000000000000000000, 1.000000000000000000 ) ) ;
#13833 = CONICAL_SURFACE ( 'NONE', #13109, 1.875500000000000167, 0.7853981633974492782 ) ;
#13835 = ORIENTED_EDGE ( 'NONE', *, *, #8944, .T. ) ;
#13834 = CARTESIAN_POINT ( 'NONE',  ( 3.874999999999999556, 3.105999999999998984, -1.130000000000000560 ) ) ;
#13836 = ORIENTED_EDGE ( 'NONE', *, *, #2500, .F. ) ;
#13837 = CARTESIAN_POINT ( 'NONE',  ( 0.6940273316166111206, 0.04143956043956045082, -0.4146485309448424417 ) ) ;
#13838 = ORIENTED_EDGE ( 'NONE', *, *, #235, .T. ) ;
#13839 = AXIS2_PLACEMENT_3D ( 'NONE', #9006, #6784, #14887 ) ;
#13840 = CARTESIAN_POINT ( 'NONE',  ( 2.889807021265107689, 0.6241886699584686671, -0.4591835166487980291 ) ) ;
#13841 = EDGE_CURVE ( 'NONE', #6416, #3063, #7708, .T. ) ;
#13842 = EDGE_CURVE ( 'NONE', #11117, #10000, #12497, .T. ) ;
#13843 = CARTESIAN_POINT ( 'NONE',  ( 2.321652452207092043, 0.05022532746090251771, 0.4077623363514504828 ) ) ;
#13844 = DIRECTION ( 'NONE',  ( -0.7071067811865436870, 8.659560562354978464E-17, -0.7071067811865512365 ) ) ;
#13845 = CARTESIAN_POINT ( 'NONE',  ( -0.7287617923574203349, -0.6590000000000000302, 0.4424999999999983391 ) ) ;
#13846 = VECTOR ( 'NONE', #1720, 39.37007874015748143 ) ;
#13847 = ORIENTED_EDGE ( 'NONE', *, *, #11892, .F. ) ;
#13848 = DIRECTION ( 'NONE',  ( 0.000000000000000000, 0.000000000000000000, 1.000000000000000000 ) ) ;
#13849 = ORIENTED_EDGE ( 'NONE', *, *, #5302, .T. ) ;
#13850 = DIRECTION ( 'NONE',  ( -0.000000000000000000, -0.000000000000000000, -1.000000000000000000 ) ) ;
#13851 = ORIENTED_EDGE ( 'NONE', *, *, #11510, .T. ) ;
#13852 = CIRCLE ( 'NONE', #11432, 2.000179419058113695 ) ;
#13853 = CARTESIAN_POINT ( 'NONE',  ( 4.315797241329101475, 3.137999999999999901, -1.570821732971949825 ) ) ;
#13854 = VERTEX_POINT ( 'NONE', #2054 ) ;
#13855 = CARTESIAN_POINT ( 'NONE',  ( 6.096491571325181269, 1.934941942652818220E-16, 1.580000000000000071 ) ) ;
#13856 = DIRECTION ( 'NONE',  ( -0.7071067811865422437, 8.659560562354996953E-17, -0.7071067811865527908 ) ) ;
#13857 = DIRECTION ( 'NONE',  ( -1.000000000000000000, -0.000000000000000000, -0.000000000000000000 ) ) ;
#13858 = AXIS2_PLACEMENT_3D ( 'NONE', #5873, #5940, #7022 ) ;
#13859 = EDGE_CURVE ( 'NONE', #5917, #2036, #10150, .T. ) ;
#13860 = CIRCLE ( 'NONE', #9250, 0.2624999999999997335 ) ;
#13861 = DIRECTION ( 'NONE',  ( 0.000000000000000000, 4.591341165822166182E-16, 1.000000000000000000 ) ) ;
#13862 = AXIS2_PLACEMENT_3D ( 'NONE', #11413, #7747, #915 ) ;
#13863 = CARTESIAN_POINT ( 'NONE',  ( 3.781227704530009337, 1.808100070518111835, -0.7963533161500825353 ) ) ;
#13864 = ORIENTED_EDGE ( 'NONE', *, *, #12454, .F. ) ;
#13865 = AXIS2_PLACEMENT_3D ( 'NONE', #11093, #3148, #1825 ) ;
#13866 = ORIENTED_EDGE ( 'NONE', *, *, #2741, .T. ) ;
#13867 = CARTESIAN_POINT ( 'NONE',  ( 3.426491571325181340, 1.958274996229347087, 0.6732298969886908457 ) ) ;
#13868 = ORIENTED_EDGE ( 'NONE', *, *, #10304, .F. ) ;
#13869 = VECTOR ( 'NONE', #9806, 39.37007874015748143 ) ;
#13870 = CARTESIAN_POINT ( 'NONE',  ( 3.388933043275772494, 0.7513023213622327390, -0.4521337140780258279 ) ) ;
#13871 = CARTESIAN_POINT ( 'NONE',  ( 2.774999999999999911, -1.679378605318041950, 1.973878605318057700 ) ) ;
#13873 = FACE_BOUND ( 'NONE', #5055, .T. ) ;
#13872 = CONICAL_SURFACE ( 'NONE', #5108, 0.2219999999999999751, 0.7853981633974349563 ) ;
#13874 = DIRECTION ( 'NONE',  ( 1.000000000000000000, 1.365923996832131609E-16, 0.000000000000000000 ) ) ;
#13875 = ORIENTED_EDGE ( 'NONE', *, *, #9302, .T. ) ;
#13876 = DIRECTION ( 'NONE',  ( 1.000000000000000000, 0.000000000000000000, 0.000000000000000000 ) ) ;
#13877 = EDGE_CURVE ( 'NONE', #10976, #9323, #14532, .T. ) ;
#13878 = CARTESIAN_POINT ( 'NONE',  ( 0.7051258599873416744, -0.02178283142415348567, -0.4764739269522892395 ) ) ;
#13879 = EDGE_CURVE ( 'NONE', #3188, #5697, #1100, .T. ) ;
#13880 = DIRECTION ( 'NONE',  ( 0.000000000000000000, 0.000000000000000000, 1.000000000000000000 ) ) ;
#13881 = AXIS2_PLACEMENT_3D ( 'NONE', #10874, #2541, #7295 ) ;
#13882 = CIRCLE ( 'NONE', #7541, 0.4070000000000022489 ) ;
#13883 = AXIS2_PLACEMENT_3D ( 'NONE', #7105, #14029, #1181 ) ;
#13884 = VECTOR ( 'NONE', #2170, 39.37007874015748143 ) ;
#13885 = EDGE_CURVE ( 'NONE', #13592, #3626, #7955, .T. ) ;
#13886 = CIRCLE ( 'NONE', #12425, 0.1249999999999999029 ) ;
#13887 = ORIENTED_EDGE ( 'NONE', *, *, #15086, .T. ) ;
#13889 = EDGE_LOOP ( 'NONE', ( #6497, #1402, #10434, #228 ) ) ;
#13888 = CARTESIAN_POINT ( 'NONE',  ( 0.3662050505264397016, 1.600827805288693062, 0.1276197524518947191 ) ) ;
#13890 = ORIENTED_EDGE ( 'NONE', *, *, #4943, .F. ) ;
#13892 = ORIENTED_EDGE ( 'NONE', *, *, #11981, .T. ) ;
#13891 = DIRECTION ( 'NONE',  ( -0.000000000000000000, -1.000000000000000000, 0.000000000000000000 ) ) ;
#13893 = ORIENTED_EDGE ( 'NONE', *, *, #5155, .T. ) ;
#13894 = B_SPLINE_CURVE_WITH_KNOTS ( 'NONE', 3,
 ( #12066, #1574, #2960, #12284, #12213, #1796, #5564, #15042, #10378, #11367, #2024, #4569, #4646, #6708, #3337, #14892, #13803, #2189, #3195, #4341, #9236, #9084, #11601, #9317, #7856, #6790, #1105, #870, #3420, #5791, #8010, #7932 ),
 .UNSPECIFIED., .F., .F.,
 ( 4, 2, 2, 2, 2, 2, 2, 2, 2, 2, 2, 2, 2, 2, 2, 4 ),
 ( 0.000000000000000000, 0.004420635650383453706, 0.006630953475575180993, 0.008841271300766907412, 0.01105158912595863470, 0.01215674803855450008, 0.01326190695115036199, 0.01768254260153383217, 0.01878770151412969755, 0.01989286042672556640, 0.02210317825191729715, 0.02431349607710902791, 0.02652381390230075867, 0.03094444955268424099, 0.03315476737787598216, 0.03536508520306772679 ),
 .UNSPECIFIED. ) ;
#13895 = CARTESIAN_POINT ( 'NONE',  ( 0.007060738305901492935, -0.2214999999999999469, -0.4999002720578262782 ) ) ;
#13896 = DIRECTION ( 'NONE',  ( 1.000000000000000000, 0.000000000000000000, 0.000000000000000000 ) ) ;
#13897 = DIRECTION ( 'NONE',  ( -1.000000000000000000, 0.000000000000000000, 1.639108796198557537E-14 ) ) ;
#13898 = ORIENTED_EDGE ( 'NONE', *, *, #13463, .F. ) ;
#13899 = CARTESIAN_POINT ( 'NONE',  ( 3.944129661530210385, 0.000000000000000000, 0.000000000000000000 ) ) ;
#13900 = CYLINDRICAL_SURFACE ( 'NONE', #1898, 2.500000000000000444 ) ;
#13901 = EDGE_CURVE ( 'NONE', #6443, #11969, #1341, .T. ) ;
#13902 = CIRCLE ( 'NONE', #4631, 0.9499999999999992895 ) ;
#13903 = CARTESIAN_POINT ( 'NONE',  ( 3.674479682832311855, 1.933833928510312328, -0.7233581415293754979 ) ) ;
#13904 = ADVANCED_FACE ( 'NONE', ( #12766 ), #12614, .F. ) ;
#13905 = CARTESIAN_POINT ( 'NONE',  ( 0.8852856429364857060, 0.1749999999999999889, -0.2372115730956926571 ) ) ;
#13906 = CARTESIAN_POINT ( 'NONE',  ( -0.4108223460329323840, 4.529999999999999361, 0.2849999999999956457 ) ) ;
#13907 = CYLINDRICAL_SURFACE ( 'NONE', #8224, 1.124999999999999556 ) ;
#13908 = DIRECTION ( 'NONE',  ( 0.000000000000000000, 0.000000000000000000, 1.000000000000000000 ) ) ;
#13909 = DIRECTION ( 'NONE',  ( -0.000000000000000000, -0.000000000000000000, -1.000000000000000000 ) ) ;
#13910 = DIRECTION ( 'NONE',  ( -1.000000000000000000, -2.130223169792495565E-16, 0.000000000000000000 ) ) ;
#13911 = LINE ( 'NONE', #6974, #12309 ) ;
#13912 = EDGE_CURVE ( 'NONE', #8675, #10024, #1834, .T. ) ;
#13913 = VECTOR ( 'NONE', #3635, 39.37007874015748143 ) ;
#13914 = DIRECTION ( 'NONE',  ( -1.000000000000000000, -0.000000000000000000, -0.000000000000000000 ) ) ;
#13916 = ORIENTED_EDGE ( 'NONE', *, *, #13841, .T. ) ;
#13915 = FACE_BOUND ( 'NONE', #984, .T. ) ;
#13917 = ORIENTED_EDGE ( 'NONE', *, *, #3855, .T. ) ;
#13918 = EDGE_CURVE ( 'NONE', #4018, #11132, #5511, .T. ) ;
#13919 = CARTESIAN_POINT ( 'NONE',  ( 3.944129661530210385, 1.867491090171841117, 0.4951980309903491473 ) ) ;
#13920 = EDGE_LOOP ( 'NONE', ( #13283, #4503, #14904, #11256 ) ) ;
#13921 = DIRECTION ( 'NONE',  ( -0.000000000000000000, -1.000000000000000000, -0.000000000000000000 ) ) ;
#13922 = CARTESIAN_POINT ( 'NONE',  ( 3.096478849372235942, 0.7064487239733228119, -0.4562644230314656935 ) ) ;
#13923 = DIRECTION ( 'NONE',  ( 0.000000000000000000, 0.000000000000000000, 1.000000000000000000 ) ) ;
#13924 = CARTESIAN_POINT ( 'NONE',  ( 0.9672769954795885639, -0.4829975555521403008, -0.4081482409674996870 ) ) ;
#13925 = ADVANCED_FACE ( 'NONE', ( #10493 ), #7965, .F. ) ;
#13926 = ORIENTED_EDGE ( 'NONE', *, *, #11946, .T. ) ;
#13927 = CARTESIAN_POINT ( 'NONE',  ( 0.7022716438625806745, -0.4145615347806886342, 0.4812718407965458356 ) ) ;
#13928 = DIRECTION ( 'NONE',  ( -0.01412288512831583534, 0.000000000000000000, -0.9999002670844989726 ) ) ;
#13929 = LINE ( 'NONE', #9365, #11204 ) ;
#13930 = ORIENTED_EDGE ( 'NONE', *, *, #5518, .F. ) ;
#13931 = AXIS2_PLACEMENT_3D ( 'NONE', #7560, #14587, #11229 ) ;
#13932 = FACE_OUTER_BOUND ( 'NONE', #8184, .T. ) ;
#13933 = ORIENTED_EDGE ( 'NONE', *, *, #8540, .T. ) ;
#13934 = ADVANCED_FACE ( 'NONE', ( #6830 ), #13078, .T. ) ;
#13935 = EDGE_CURVE ( 'NONE', #1992, #2828, #13990, .T. ) ;
#13936 = CARTESIAN_POINT ( 'NONE',  ( 2.774999999999999911, 1.575000000000016609, 1.575000000000000178 ) ) ;
#13937 = ORIENTED_EDGE ( 'NONE', *, *, #11759, .F. ) ;
#13938 = DIRECTION ( 'NONE',  ( 0.000000000000000000, 0.000000000000000000, -1.000000000000000000 ) ) ;
#13939 = DIRECTION ( 'NONE',  ( -1.000000000000000000, -0.000000000000000000, -0.000000000000000000 ) ) ;
#13940 = CYLINDRICAL_SURFACE ( 'NONE', #8279, 1.000000000000000444 ) ;
#13941 = AXIS2_PLACEMENT_3D ( 'NONE', #14165, #7151, #2544 ) ;
#13942 = CARTESIAN_POINT ( 'NONE',  ( 0.06299999999999994493, 0.000000000000000000, 0.000000000000000000 ) ) ;
#13943 = DIRECTION ( 'NONE',  ( 0.7071067811865607844, -0.7071067811865343611, -1.170732267570243064E-16 ) ) ;
#13944 = CARTESIAN_POINT ( 'NONE',  ( 3.809126238595077485, 1.878820374380962832, -0.7477401187409083994 ) ) ;
#13945 = EDGE_LOOP ( 'NONE', ( #3453, #1547, #7651, #7453 ) ) ;
#13946 = ORIENTED_EDGE ( 'NONE', *, *, #6553, .F. ) ;
#13947 = EDGE_CURVE ( 'NONE', #12193, #4855, #12823, .T. ) ;
#13948 = DIRECTION ( 'NONE',  ( -0.000000000000000000, 1.000000000000000000, -0.000000000000000000 ) ) ;
#13949 = ORIENTED_EDGE ( 'NONE', *, *, #5733, .F. ) ;
#13950 = CIRCLE ( 'NONE', #2730, 0.5000000000000002220 ) ;
#13951 = CARTESIAN_POINT ( 'NONE',  ( 2.001999999999999780, 0.000000000000000000, -1.409999999999999920 ) ) ;
#13952 = CARTESIAN_POINT ( 'NONE',  ( 3.875000000000000000, 3.137999999999999901, 0.5000000000000002220 ) ) ;
#13953 = DIRECTION ( 'NONE',  ( 0.000000000000000000, -0.7071067811865587860, -0.7071067811865362485 ) ) ;
#13954 = DIRECTION ( 'NONE',  ( 0.000000000000000000, 0.000000000000000000, -1.000000000000000000 ) ) ;
#13955 = ORIENTED_EDGE ( 'NONE', *, *, #10322, .T. ) ;
#13956 = CARTESIAN_POINT ( 'NONE',  ( 4.344846310392954436, 3.567999999999999616, 1.491010071662831393 ) ) ;
#13957 = CARTESIAN_POINT ( 'NONE',  ( 0.6867276282385254005, 0.03909868245979658541, -0.4280639610650152638 ) ) ;
#13958 = LINE ( 'NONE', #5877, #11512 ) ;
#13959 = CARTESIAN_POINT ( 'NONE',  ( 2.372634528609593119, 0.1852128444980909450, -0.4664882128727458888 ) ) ;
#13960 = AXIS2_PLACEMENT_3D ( 'NONE', #10232, #6566, #955 ) ;
#13961 = CARTESIAN_POINT ( 'NONE',  ( 4.626489205401124849, 1.810545309228444255, 0.03721021400973596044 ) ) ;
#13962 = EDGE_LOOP ( 'NONE', ( #3109, #9823, #14593, #1330 ) ) ;
#13964 = VERTEX_POINT ( 'NONE', #3372 ) ;
#13963 = FACE_OUTER_BOUND ( 'NONE', #4053, .T. ) ;
#13965 = ORIENTED_EDGE ( 'NONE', *, *, #14266, .F. ) ;
#13967 = ORIENTED_EDGE ( 'NONE', *, *, #6525, .T. ) ;
#13966 = DIRECTION ( 'NONE',  ( 1.000000000000000000, 0.000000000000000000, 0.000000000000000000 ) ) ;
#13968 = ORIENTED_EDGE ( 'NONE', *, *, #2947, .T. ) ;
#13969 = CIRCLE ( 'NONE', #5695, 0.05999999999999997696 ) ;
#13970 = DIRECTION ( 'NONE',  ( -1.000000000000000000, -0.000000000000000000, -0.000000000000000000 ) ) ;
#13971 = CARTESIAN_POINT ( 'NONE',  ( 2.774999999999999911, 0.000000000000000000, 0.000000000000000000 ) ) ;
#13972 = ORIENTED_EDGE ( 'NONE', *, *, #3989, .F. ) ;
#13973 = CARTESIAN_POINT ( 'NONE',  ( 0.09500000000000431710, 1.679378605318059492, 1.679378605318041506 ) ) ;
#13974 = CARTESIAN_POINT ( 'NONE',  ( 0.6555297760382666761, -0.4026665662008522828, -0.5099209754895143165 ) ) ;
#13975 = DIRECTION ( 'NONE',  ( 8.659560562354890950E-17, 0.7071067811865509034, -0.7071067811865441310 ) ) ;
#13976 = AXIS2_PLACEMENT_3D ( 'NONE', #15048, #7114, #14969 ) ;
#13977 = CYLINDRICAL_SURFACE ( 'NONE', #10354, 0.06000000000000001166 ) ;
#13978 = AXIS2_PLACEMENT_3D ( 'NONE', #3125, #10089, #4040 ) ;
#13979 = FACE_OUTER_BOUND ( 'NONE', #1640, .T. ) ;
#13980 = CIRCLE ( 'NONE', #11808, 0.2944999999999856066 ) ;
#13981 = DIRECTION ( 'NONE',  ( 0.000000000000000000, 0.000000000000000000, 1.000000000000000000 ) ) ;
#13982 = CARTESIAN_POINT ( 'NONE',  ( 3.874999999999999556, 3.137999999999999901, -1.320000000000000062 ) ) ;
#13983 = CARTESIAN_POINT ( 'NONE',  ( 8.475037399843312613, 0.9289129992088659415, 0.3802960819231170908 ) ) ;
#13984 = ADVANCED_FACE ( 'NONE', ( #3606 ), #5035, .F. ) ;
#13985 = CARTESIAN_POINT ( 'NONE',  ( 4.679414359322546346, 1.732195860677045118, -0.09958524941061751290 ) ) ;
#13986 = EDGE_CURVE ( 'NONE', #2564, #10875, #111, .T. ) ;
#13987 = ORIENTED_EDGE ( 'NONE', *, *, #4145, .F. ) ;
#13988 = ADVANCED_FACE ( 'NONE', ( #1138 ), #9679, .F. ) ;
#13989 = AXIS2_PLACEMENT_3D ( 'NONE', #3271, #10240, #798 ) ;
#13990 = LINE ( 'NONE', #3523, #840 ) ;
#13992 = ORIENTED_EDGE ( 'NONE', *, *, #15049, .F. ) ;
#13991 = DIRECTION ( 'NONE',  ( 0.000000000000000000, 0.000000000000000000, -1.000000000000000000 ) ) ;
#13993 = ORIENTED_EDGE ( 'NONE', *, *, #13245, .T. ) ;
#13994 = DIRECTION ( 'NONE',  ( 0.000000000000000000, 0.000000000000000000, -1.000000000000000000 ) ) ;
#13995 = EDGE_LOOP ( 'NONE', ( #5359, #9610 ) ) ;
#13996 = CARTESIAN_POINT ( 'NONE',  ( 3.876560711617219379, 3.137999999999999901, 0.000000000000000000 ) ) ;
#13997 = EDGE_CURVE ( 'NONE', #6090, #6131, #10563, .T. ) ;
#13998 = ADVANCED_FACE ( 'NONE', ( #4520 ), #9909, .T. ) ;
#13999 = DIRECTION ( 'NONE',  ( 0.000000000000000000, 2.708891287835076134E-14, 1.000000000000000000 ) ) ;
#14000 = CIRCLE ( 'NONE', #4981, 0.3190000000000000058 ) ;
#14001 = CARTESIAN_POINT ( 'NONE',  ( 0.6500000000000001332, 1.679378605318035733, -1.679378605318065487 ) ) ;
#14002 = AXIS2_PLACEMENT_3D ( 'NONE', #10270, #7889, #3077 ) ;
#14003 = ORIENTED_EDGE ( 'NONE', *, *, #8783, .F. ) ;
#14004 = CARTESIAN_POINT ( 'NONE',  ( 3.521940692902104431, 2.009083282330886622, -0.6610767032427503631 ) ) ;
#14005 = FACE_OUTER_BOUND ( 'NONE', #3852, .T. ) ;
#14006 = DIRECTION ( 'NONE',  ( 0.000000000000000000, 0.000000000000000000, 1.000000000000000000 ) ) ;
#14007 = ORIENTED_EDGE ( 'NONE', *, *, #13788, .F. ) ;
#14008 = LINE ( 'NONE', #8379, #9439 ) ;
#14009 = ORIENTED_EDGE ( 'NONE', *, *, #12511, .F. ) ;
#14010 = LINE ( 'NONE', #5541, #8837 ) ;
#14011 = CARTESIAN_POINT ( 'NONE',  ( 0.2099999999999999922, 1.239999999999999991, 0.3809527529760087239 ) ) ;
#14012 = ORIENTED_EDGE ( 'NONE', *, *, #1396, .T. ) ;
#14013 = VECTOR ( 'NONE', #10324, 39.37007874015748143 ) ;
#14014 = AXIS2_PLACEMENT_3D ( 'NONE', #11793, #5677, #11727 ) ;
#14015 = CARTESIAN_POINT ( 'NONE',  ( 2.807000000000000828, 1.679378605318042395, -1.941878605318058337 ) ) ;
#14016 = DIRECTION ( 'NONE',  ( 0.000000000000000000, 0.000000000000000000, -1.000000000000000000 ) ) ;
#14017 = EDGE_CURVE ( 'NONE', #8556, #14201, #9425, .T. ) ;
#14018 = FACE_OUTER_BOUND ( 'NONE', #11835, .T. ) ;
#14019 = EDGE_CURVE ( 'NONE', #2400, #8556, #5261, .T. ) ;
#14020 = CIRCLE ( 'NONE', #815, 0.06000000000000003941 ) ;
#14021 = CARTESIAN_POINT ( 'NONE',  ( 6.826491571325181695, -1.679378605318047946, -1.679378605318053497 ) ) ;
#14022 = PRODUCT_DEFINITION_FORMATION_WITH_SPECIFIED_SOURCE ( 'ANY', '', #8859, .NOT_KNOWN. ) ;
#14023 = ORIENTED_EDGE ( 'NONE', *, *, #14263, .T. ) ;
#14024 = ORIENTED_EDGE ( 'NONE', *, *, #8126, .F. ) ;
#14025 = CARTESIAN_POINT ( 'NONE',  ( 3.426491571325181340, 2.038142229251666215, 0.6032823416034359676 ) ) ;
#14026 = VERTEX_POINT ( 'NONE', #15074 ) ;
#14027 = CARTESIAN_POINT ( 'NONE',  ( 2.124999999999999556, 0.000000000000000000, -1.875000000000000000 ) ) ;
#14028 = PLANE ( 'NONE',  #5419 ) ;
#14029 = DIRECTION ( 'NONE',  ( -0.000000000000000000, -1.000000000000000000, -0.000000000000000000 ) ) ;
#14030 = CIRCLE ( 'NONE', #1815, 0.07500000000000002498 ) ;
#14031 = CARTESIAN_POINT ( 'NONE',  ( 0.7238772453881179292, -0.005046247197760479232, -0.4547576871318953495 ) ) ;
#14032 = ORIENTED_EDGE ( 'NONE', *, *, #6771, .F. ) ;
#14033 = DIRECTION ( 'NONE',  ( 0.000000000000000000, 1.000000000000000000, 0.000000000000000000 ) ) ;
#14034 = CIRCLE ( 'NONE', #9419, 0.9999999999999998890 ) ;
#14035 = AXIS2_PLACEMENT_3D ( 'NONE', #8137, #2539, #11646 ) ;
#14036 = CARTESIAN_POINT ( 'NONE',  ( 2.774999999999999911, -2.360000000000016751, -1.574999999999999956 ) ) ;
#14037 = CARTESIAN_POINT ( 'NONE',  ( 0.6975252985509352577, 1.829624391447200865E-16, -1.494001693158432786 ) ) ;
#14038 = EDGE_CURVE ( 'NONE', #8178, #6882, #7238, .T. ) ;
#14039 = FACE_OUTER_BOUND ( 'NONE', #14826, .T. ) ;
#14040 = AXIS2_PLACEMENT_3D ( 'NONE', #6730, #13742, #9099 ) ;
#14041 = CARTESIAN_POINT ( 'NONE',  ( 4.670780491554178404, 1.730766616691212123, 0.1519652760568382388 ) ) ;
#14042 = ORIENTED_EDGE ( 'NONE', *, *, #8797, .F. ) ;
#14044 = ORIENTED_EDGE ( 'NONE', *, *, #7394, .T. ) ;
#14043 = CYLINDRICAL_SURFACE ( 'NONE', #9124, 1.000000000000000888 ) ;
#14045 = ORIENTED_EDGE ( 'NONE', *, *, #5028, .T. ) ;
#14046 = DIRECTION ( 'NONE',  ( 0.000000000000000000, -1.000000000000000000, 0.000000000000000000 ) ) ;
#14047 = ORIENTED_EDGE ( 'NONE', *, *, #3562, .F. ) ;
#14048 = DIRECTION ( 'NONE',  ( -1.000000000000000000, -0.000000000000000000, -0.000000000000000000 ) ) ;
#14049 =( NAMED_UNIT ( * ) PLANE_ANGLE_UNIT ( ) SI_UNIT ( $, .RADIAN. ) );
#14050 = FACE_BOUND ( 'NONE', #10447, .T. ) ;
#14051 = ORIENTED_EDGE ( 'NONE', *, *, #1300, .T. ) ;
#14052 = CARTESIAN_POINT ( 'NONE',  ( 2.061999999999999389, 1.726751986797767896E-16, 1.409999999999999920 ) ) ;
#14053 = FACE_BOUND ( 'NONE', #36, .T. ) ;
#14054 = AXIS2_PLACEMENT_3D ( 'NONE', #4930, #1156, #11806 ) ;
#14055 = CARTESIAN_POINT ( 'NONE',  ( 3.875000000000000000, 3.170499999999999208, 0.000000000000000000 ) ) ;
#14056 = FACE_BOUND ( 'NONE', #8564, .T. ) ;
#14057 = VECTOR ( 'NONE', #6570, 39.37007874015748854 ) ;
#14058 = AXIS2_PLACEMENT_3D ( 'NONE', #2491, #13948, #11897 ) ;
#14059 = EDGE_CURVE ( 'NONE', #2897, #3063, #11124, .T. ) ;
#14060 = DIRECTION ( 'NONE',  ( -1.000000000000000000, -0.000000000000000000, -0.000000000000000000 ) ) ;
#14061 = DIRECTION ( 'NONE',  ( 0.000000000000000000, 0.000000000000000000, 1.000000000000000000 ) ) ;
#14062 = CARTESIAN_POINT ( 'NONE',  ( 3.743770895704081614, 0.8757747662568124980, 0.4827512383967037524 ) ) ;
#14063 = CYLINDRICAL_SURFACE ( 'NONE', #8182, 1.000000000000000000 ) ;
#14064 = CIRCLE ( 'NONE', #5272, 0.2219999999999999751 ) ;
#14065 = ORIENTED_EDGE ( 'NONE', *, *, #356, .T. ) ;
#14066 = DIRECTION ( 'NONE',  ( -0.000000000000000000, -1.000000000000000000, -0.000000000000000000 ) ) ;
#14068 = ORIENTED_EDGE ( 'NONE', *, *, #8245, .T. ) ;
#14067 = CYLINDRICAL_SURFACE ( 'NONE', #3819, 1.000000000000000000 ) ;
#14069 = EDGE_LOOP ( 'NONE', ( #12090, #6576, #4418, #11133 ) ) ;
#14070 = AXIS2_PLACEMENT_3D ( 'NONE', #12954, #4634, #1167 ) ;
#14071 = TOROIDAL_SURFACE ( 'NONE', #11392, 0.3439999999999999170, 0.1068000000000000754 ) ;
#14072 = DIRECTION ( 'NONE',  ( 1.000000000000000000, 0.000000000000000000, 0.000000000000000000 ) ) ;
#14073 = DIRECTION ( 'NONE',  ( -1.000000000000000000, -0.000000000000000000, -0.000000000000000000 ) ) ;
#14074 = CARTESIAN_POINT ( 'NONE',  ( 2.917021349547979536, 0.5710164562863511151, 0.4587991334809356503 ) ) ;
#14075 = ORIENTED_EDGE ( 'NONE', *, *, #2823, .T. ) ;
#14076 = DIRECTION ( 'NONE',  ( -0.000000000000000000, -1.000000000000000000, -0.000000000000000000 ) ) ;
#14077 =( REPRESENTATION_RELATIONSHIP ('NONE','NONE', #3591, #8950 ) REPRESENTATION_RELATIONSHIP_WITH_TRANSFORMATION ( #3030 )SHAPE_REPRESENTATION_RELATIONSHIP( ) );
#14078 = EDGE_CURVE ( 'NONE', #14557, #2844, #11977, .T. ) ;
#14079 = ADVANCED_FACE ( 'NONE', ( #14293 ), #13284, .F. ) ;
#14080 = AXIS2_PLACEMENT_3D ( 'NONE', #11303, #12375, #1967 ) ;
#14081 = LINE ( 'NONE', #3616, #12334 ) ;
#14082 = EDGE_CURVE ( 'NONE', #1005, #2093, #12345, .T. ) ;
#14083 = DIRECTION ( 'NONE',  ( 0.03489949670248613384, -0.9993908270190963172, 0.000000000000000000 ) ) ;
#14084 = ORIENTED_EDGE ( 'NONE', *, *, #2107, .F. ) ;
#14085 = CARTESIAN_POINT ( 'NONE',  ( 0.000000000000000000, 1.591999999999999638, -0.2812500000000000555 ) ) ;
#14086 = CONICAL_SURFACE ( 'NONE', #2853, 0.06999999999999829969, 0.7853981633974298493 ) ;
#14087 = FACE_OUTER_BOUND ( 'NONE', #14509, .T. ) ;
#14088 = DIRECTION ( 'NONE',  ( 0.000000000000000000, 1.000000000000000000, 0.000000000000000000 ) ) ;
#14089 = ORIENTED_EDGE ( 'NONE', *, *, #13879, .F. ) ;
#14090 = EDGE_CURVE ( 'NONE', #2897, #7967, #7282, .T. ) ;
#14091 = PLANE ( 'NONE',  #9675 ) ;
#14092 = VERTEX_POINT ( 'NONE', #2749 ) ;
#14093 = AXIS2_PLACEMENT_3D ( 'NONE', #11989, #1497, #332 ) ;
#14094 = DIRECTION ( 'NONE',  ( 1.000000000000000000, 0.000000000000000000, 0.000000000000000000 ) ) ;
#14095 = EDGE_LOOP ( 'NONE', ( #3009, #217, #12376, #4082 ) ) ;
#14096 =( BOUNDED_CURVE ( )  B_SPLINE_CURVE ( 3, ( #11782, #3516, #10257, #5741 ),
 .UNSPECIFIED., .F., .F. ) 
 B_SPLINE_CURVE_WITH_KNOTS ( ( 4, 4 ),
 ( 0.000000000000000000, 1.556672972142351341 ),
 .UNSPECIFIED. ) 
 CURVE ( )  GEOMETRIC_REPRESENTATION_ITEM ( )  RATIONAL_B_SPLINE_CURVE ( ( 1.000000000000000000, 0.8080549792898082950, 0.8080549792898082950, 1.000000000000000000 ) ) 
 REPRESENTATION_ITEM ( '' )  );
#14097 = DIRECTION ( 'NONE',  ( -1.000000000000000000, -0.000000000000000000, -0.000000000000000000 ) ) ;
#14098 = CARTESIAN_POINT ( 'NONE',  ( 8.469665986256828205, 0.9969999999999998863, 6.829619984160658046E-17 ) ) ;
#14099 = EDGE_CURVE ( 'NONE', #13668, #5653, #8639, .T. ) ;
#14100 = CARTESIAN_POINT ( 'NONE',  ( 3.405153689607044232, 3.567999999999999616, -1.491010071662831171 ) ) ;
#14101 = DIRECTION ( 'NONE',  ( 0.000000000000000000, 0.000000000000000000, -1.000000000000000000 ) ) ;
#14102 = ORIENTED_EDGE ( 'NONE', *, *, #1801, .T. ) ;
#14103 = ORIENTED_EDGE ( 'NONE', *, *, #10363, .T. ) ;
#14104 = AXIS2_PLACEMENT_3D ( 'NONE', #10250, #2123, #810 ) ;
#14105 = ORIENTED_EDGE ( 'NONE', *, *, #1455, .F. ) ;
#14106 = EDGE_CURVE ( 'NONE', #2690, #7890, #3087, .T. ) ;
#14107 = UNCERTAINTY_MEASURE_WITH_UNIT (LENGTH_MEASURE( 1.000000000000000082E-05 ), #1449, 'distance_accuracy_value', 'NONE');
#14108 = CARTESIAN_POINT ( 'NONE',  ( -0.7287617923574203349, -0.6590000000000000302, -0.4424999999999983391 ) ) ;
#14109 = CARTESIAN_POINT ( 'NONE',  ( 3.085497600961857767, 0.7407061222255643118, -0.4564195254101433008 ) ) ;
#14110 = FACE_OUTER_BOUND ( 'NONE', #7987, .T. ) ;
#14111 = EDGE_CURVE ( 'NONE', #8303, #7967, #2339, .T. ) ;
#14112 = LINE ( 'NONE', #11827, #2647 ) ;
#14113 = VERTEX_POINT ( 'NONE', #2682 ) ;
#14114 = DIRECTION ( 'NONE',  ( 0.000000000000000000, 0.000000000000000000, -1.000000000000000000 ) ) ;
#14115 = AXIS2_PLACEMENT_3D ( 'NONE', #9603, #10814, #7311 ) ;
#14116 = CARTESIAN_POINT ( 'NONE',  ( 1.775981552640430561, 0.05988294188167953003, 0.4749155147932142551 ) ) ;
#14117 = CARTESIAN_POINT ( 'NONE',  ( 6.176491571325181340, -1.679378605318047946, -1.272378605318051248 ) ) ;
#14118 = AXIS2_PLACEMENT_3D ( 'NONE', #886, #966, #806 ) ;
#14119 = VECTOR ( 'NONE', #6293, 39.37007874015748143 ) ;
#14120 = CIRCLE ( 'NONE', #2889, 2.070731779878276502 ) ;
#14121 = LENGTH_MEASURE_WITH_UNIT ( LENGTH_MEASURE( 0.02539999999999999897 ), #15125 );
#14122 = CIRCLE ( 'NONE', #10956, 2.500000000000000444 ) ;
#14123 = CARTESIAN_POINT ( 'NONE',  ( 4.613342449693359271, 1.747135830664880540, 0.1413303526058345416 ) ) ;
#14124 = ORIENTED_EDGE ( 'NONE', *, *, #14539, .F. ) ;
#14126 = EDGE_LOOP ( 'NONE', ( #3315, #1310, #10244, #266 ) ) ;
#14125 = CARTESIAN_POINT ( 'NONE',  ( 0.3117416060218692886, 1.602949672542214321, 0.2219532054890206441 ) ) ;
#14127 = CIRCLE ( 'NONE', #12658, 0.2812500000000000555 ) ;
#14128 = ORIENTED_EDGE ( 'NONE', *, *, #14687, .F. ) ;
#14129 = CARTESIAN_POINT ( 'NONE',  ( 0.6179999999999965521, 1.679378605318059492, 1.679378605318041506 ) ) ;
#14130 = EDGE_LOOP ( 'NONE', ( #12113, #14068, #8752, #11616 ) ) ;
#14131 = ADVANCED_FACE ( 'NONE', ( #1515 ), #7419, .F. ) ;
#14132 = FACE_OUTER_BOUND ( 'NONE', #8004, .T. ) ;
#14133 = EDGE_CURVE ( 'NONE', #6033, #1534, #12076, .T. ) ;
#14134 = APPLICATION_PROTOCOL_DEFINITION ( 'draft international standard', 'automotive_design', 1998, #6858 ) ;
#14135 = DIRECTION ( 'NONE',  ( 0.000000000000000000, 0.000000000000000000, -1.000000000000000000 ) ) ;
#14136 = ORIENTED_EDGE ( 'NONE', *, *, #2931, .F. ) ;
#14137 = CARTESIAN_POINT ( 'NONE',  ( 3.426491571325181340, -2.400000000000011902, -0.6999999999999596545 ) ) ;
#14138 = CARTESIAN_POINT ( 'NONE',  ( 3.426491571325181340, -1.575000000000027489, -1.574999999999989297 ) ) ;
#14139 = VECTOR ( 'NONE', #13278, 39.37007874015748143 ) ;
#14140 = CARTESIAN_POINT ( 'NONE',  ( 3.713865648090597826, 1.916531464605631507, 0.7332543789835506143 ) ) ;
#14141 = AXIS2_PLACEMENT_3D ( 'NONE', #3623, #9444, #1306 ) ;
#14142 = DIRECTION ( 'NONE',  ( -0.4999999999999998335, 0.000000000000000000, -0.8660254037844385966 ) ) ;
#14143 = VECTOR ( 'NONE', #9566, 39.37007874015748854 ) ;
#14144 = CIRCLE ( 'NONE', #1185, 0.8653656741516848605 ) ;
#14145 = CARTESIAN_POINT ( 'NONE',  ( 8.476283996537762988, 0.8689495495877206377, 0.3203020658980472168 ) ) ;
#14146 = CARTESIAN_POINT ( 'NONE',  ( 3.874999999999999556, 3.535499999999999421, 1.130000000000000560 ) ) ;
#14147 = CARTESIAN_POINT ( 'NONE',  ( 3.875000000000000000, 0.8660254037844384856, 0.5000000000000002220 ) ) ;
#14148 = FACE_BOUND ( 'NONE', #4546, .T. ) ;
#14149 = VERTEX_POINT ( 'NONE', #5974 ) ;
#14150 = PRESENTATION_LAYER_ASSIGNMENT (  '', '', ( #6345 ) ) ;
#14151 = FACE_OUTER_BOUND ( 'NONE', #7547, .T. ) ;
#14153 = VERTEX_POINT ( 'NONE', #1587 ) ;
#14152 = CARTESIAN_POINT ( 'NONE',  ( 6.794491571325179891, -1.679378605318047946, -1.679378605318053497 ) ) ;
#14154 = ORIENTED_EDGE ( 'NONE', *, *, #13547, .F. ) ;
#14155 = CARTESIAN_POINT ( 'NONE',  ( 0.4349147617188413584, 0.7512260236060024354, -0.008611041693277364170 ) ) ;
#14156 = EDGE_CURVE ( 'NONE', #1198, #4697, #1845, .T. ) ;
#14157 = CARTESIAN_POINT ( 'NONE',  ( 3.920919094826833984, 1.873066083652677793, 0.4984382268710150776 ) ) ;
#14158 = CARTESIAN_POINT ( 'NONE',  ( 6.794491571325179891, 1.679378605318035733, -1.679378605318065487 ) ) ;
#14159 = ORIENTED_EDGE ( 'NONE', *, *, #2307, .F. ) ;
#14160 = PLANE ( 'NONE',  #12902 ) ;
#14161 = DIRECTION ( 'NONE',  ( -0.000000000000000000, 1.000000000000000000, -0.000000000000000000 ) ) ;
#14162 = CARTESIAN_POINT ( 'NONE',  ( 0.9652705920801475381, -0.4828330467331339304, -0.4119425203458965679 ) ) ;
#14163 = AXIS2_PLACEMENT_3D ( 'NONE', #14098, #12874, #4630 ) ;
#14164 = ORIENTED_EDGE ( 'NONE', *, *, #5314, .F. ) ;
#14165 = CARTESIAN_POINT ( 'NONE',  ( 3.874999999999999556, 2.750000000000000000, -1.320000000000000062 ) ) ;
#14166 = CARTESIAN_POINT ( 'NONE',  ( 3.528591654644219311, 1.932956604557751534, -0.6650985988073745414 ) ) ;
#14167 = DIRECTION ( 'NONE',  ( 0.000000000000000000, 1.000000000000000000, 0.000000000000000000 ) ) ;
#14168 = DIRECTION ( 'NONE',  ( -1.000000000000000000, -0.000000000000000000, -0.000000000000000000 ) ) ;
#14169 = EDGE_LOOP ( 'NONE', ( #300, #110, #6279, #1184 ) ) ;
#14170 = CARTESIAN_POINT ( 'NONE',  ( 2.124999999999999556, 2.360000000000015863, 1.574999999999999956 ) ) ;
#14171 = ORIENTED_EDGE ( 'NONE', *, *, #2021, .F. ) ;
#14172 = EDGE_CURVE ( 'NONE', #14996, #3585, #10638, .T. ) ;
#14173 = CARTESIAN_POINT ( 'NONE',  ( 3.426491571325181340, 1.679378605318042395, -1.679378605318058604 ) ) ;
#14174 = EDGE_LOOP ( 'NONE', ( #7184, #6748, #8406, #10147, #1247, #13955, #465, #4044, #4713, #1757, #4179, #9916 ) ) ;
#14175 = CARTESIAN_POINT ( 'NONE',  ( 3.898074040635628457, 1.878528703211115092, -0.5000000000000002220 ) ) ;
#14176 = CARTESIAN_POINT ( 'NONE',  ( 0.7983174577546989781, -0.4429999999999998939, -0.4287183451209413132 ) ) ;
#14177 = FACE_OUTER_BOUND ( 'NONE', #14751, .T. ) ;
#14178 = DIRECTION ( 'NONE',  ( 1.775701195881770796E-15, 0.000000000000000000, -1.000000000000000000 ) ) ;
#14179 = VERTEX_POINT ( 'NONE', #4831 ) ;
#14180 = ORIENTED_EDGE ( 'NONE', *, *, #1311, .F. ) ;
#14181 = ADVANCED_FACE ( 'NONE', ( #14151 ), #3687, .T. ) ;
#14182 = ORIENTED_EDGE ( 'NONE', *, *, #12563, .F. ) ;
#14183 = ADVANCED_FACE ( 'NONE', ( #12571 ), #862, .F. ) ;
#14184 = FACE_OUTER_BOUND ( 'NONE', #12260, .T. ) ;
#14185 = EDGE_CURVE ( 'NONE', #12765, #5558, #124, .T. ) ;
#14186 = CARTESIAN_POINT ( 'NONE',  ( 0.4021230921906648881, 1.589827634136293577, -0.06540787938108565125 ) ) ;
#14187 = CARTESIAN_POINT ( 'NONE',  ( 0.9318415243661355429, -0.4679825767129147662, -0.4432104562656360991 ) ) ;
#14188 = FACE_OUTER_BOUND ( 'NONE', #7251, .T. ) ;
#14189 = ORIENTED_EDGE ( 'NONE', *, *, #14705, .T. ) ;
#14190 = AXIS2_PLACEMENT_3D ( 'NONE', #3121, #7785, #12443 ) ;
#14191 = DIRECTION ( 'NONE',  ( 1.000000000000000000, 0.000000000000000000, 0.000000000000000000 ) ) ;
#14192 = ADVANCED_FACE ( 'NONE', ( #946 ), #1111, .T. ) ;
#14193 = CARTESIAN_POINT ( 'NONE',  ( 1.250847373107698557, -0.05999999999999990757, 0.4823326642216426707 ) ) ;
#14194 = DIRECTION ( 'NONE',  ( 0.000000000000000000, 1.000000000000000000, -0.000000000000000000 ) ) ;
#14195 = EDGE_CURVE ( 'NONE', #392, #13214, #4114, .T. ) ;
#14196 = AXIS2_PLACEMENT_3D ( 'NONE', #1634, #3021, #7767 ) ;
#14197 = CARTESIAN_POINT ( 'NONE',  ( 4.394406145971391453, 1.728430255068499788, -0.5437684957058670498 ) ) ;
#14198 = ORIENTED_EDGE ( 'NONE', *, *, #8012, .F. ) ;
#14200 = VERTEX_POINT ( 'NONE', #11006 ) ;
#14199 = DIRECTION ( 'NONE',  ( 0.000000000000000000, 0.000000000000000000, 1.000000000000000000 ) ) ;
#14201 = VERTEX_POINT ( 'NONE', #13793 ) ;
#14202 = DIRECTION ( 'NONE',  ( -1.000000000000000000, -0.000000000000000000, -0.000000000000000000 ) ) ;
#14203 = EDGE_LOOP ( 'NONE', ( #1428, #8025, #12323, #8227 ) ) ;
#14204 = DIRECTION ( 'NONE',  ( -1.000000000000000000, -0.000000000000000000, -0.000000000000000000 ) ) ;
#14205 = DIRECTION ( 'NONE',  ( -0.000000000000000000, -1.000000000000000000, 0.000000000000000000 ) ) ;
#14206 = EDGE_LOOP ( 'NONE', ( #11171, #223, #3769, #14964, #8736, #10820, #7930, #2202 ) ) ;
#14207 = CARTESIAN_POINT ( 'NONE',  ( 3.874999999999999556, 3.137999999999999901, 1.320000000000000062 ) ) ;
#14208 = LINE ( 'NONE', #3594, #11956 ) ;
#14209 = EDGE_CURVE ( 'NONE', #5886, #12434, #2095, .T. ) ;
#14210 = DIRECTION ( 'NONE',  ( -1.000000000000000000, -0.000000000000000000, -0.000000000000000000 ) ) ;
#14211 = VECTOR ( 'NONE', #14481, 39.37007874015748143 ) ;
#14212 = EDGE_CURVE ( 'NONE', #10807, #6236, #7009, .T. ) ;
#14213 = PRODUCT_DEFINITION_SHAPE ( 'NONE', 'NONE',  #14914 ) ;
#14214 = DIRECTION ( 'NONE',  ( 0.000000000000000000, 0.000000000000000000, -1.000000000000000000 ) ) ;
#14215 = FACE_OUTER_BOUND ( 'NONE', #3429, .T. ) ;
#14216 = EDGE_CURVE ( 'NONE', #1024, #7355, #6865, .T. ) ;
#14217 = CARTESIAN_POINT ( 'NONE',  ( 3.462756589970257703, 1.936639940275549199, 0.7054686714132032410 ) ) ;
#14218 = CARTESIAN_POINT ( 'NONE',  ( 4.675740426773506542, 1.731584457788192921, -0.1243058436455859866 ) ) ;
#14219 = ADVANCED_BREP_SHAPE_REPRESENTATION ( '', ( #10334, #8424 ), #9874 ) ;
#14220 = ORIENTED_EDGE ( 'NONE', *, *, #14106, .F. ) ;
#14221 = CARTESIAN_POINT ( 'NONE',  ( 0.7017867892446606470, -0.4844395604395603239, 0.4010711782184315233 ) ) ;
#14223 = ORIENTED_EDGE ( 'NONE', *, *, #12791, .F. ) ;
#14222 = CARTESIAN_POINT ( 'NONE',  ( 6.826491571325181695, 1.679378605318059492, 1.679378605318041506 ) ) ;
#14224 = EDGE_LOOP ( 'NONE', ( #13671, #5231 ) ) ;
#14225 = CARTESIAN_POINT ( 'NONE',  ( 3.874999999999999556, 3.535499999999999421, -1.509999999999999787 ) ) ;
#14226 = DIRECTION ( 'NONE',  ( -0.000000000000000000, -1.000000000000000000, -0.000000000000000000 ) ) ;
#14227 = ORIENTED_EDGE ( 'NONE', *, *, #1551, .T. ) ;
#14228 = DIRECTION ( 'NONE',  ( -1.000000000000000000, 0.000000000000000000, 0.000000000000000000 ) ) ;
#14229 = VECTOR ( 'NONE', #12782, 39.37007874015748143 ) ;
#14230 = DIRECTION ( 'NONE',  ( -1.655665450705613915E-16, -3.103226861728128995E-32, -1.000000000000000000 ) ) ;
#14231 = CARTESIAN_POINT ( 'NONE',  ( -0.1807106342563527812, 1.379999999999999671, 3.262375646219079751E-17 ) ) ;
#14232 = ORIENTED_EDGE ( 'NONE', *, *, #12596, .T. ) ;
#14233 = EDGE_CURVE ( 'NONE', #8835, #7260, #3324, .T. ) ;
#14234 = DIRECTION ( 'NONE',  ( -1.000000000000000000, -0.000000000000000000, -0.000000000000000000 ) ) ;
#14235 = CARTESIAN_POINT ( 'NONE',  ( 2.500728763858891129E-17, 0.000000000000000000, -0.2041999999999996596 ) ) ;
#14236 = DIRECTION ( 'NONE',  ( 1.000000000000000000, 0.000000000000000000, -1.224646799147353207E-16 ) ) ;
#14237 = CARTESIAN_POINT ( 'NONE',  ( -6.123233995736766036E-17, 0.000000000000000000, 0.000000000000000000 ) ) ;
#14238 = ORIENTED_EDGE ( 'NONE', *, *, #5256, .F. ) ;
#14239 = CARTESIAN_POINT ( 'NONE',  ( 3.875000000000000000, 3.137999999999999901, 0.5174999999999995159 ) ) ;
#14240 = ORIENTED_EDGE ( 'NONE', *, *, #8746, .F. ) ;
#14241 = CARTESIAN_POINT ( 'NONE',  ( 0.7007556580885032638, -0.04192514642889976634, 0.4875099722676214387 ) ) ;
#14242 = ORIENTED_EDGE ( 'NONE', *, *, #2359, .F. ) ;
#14243 = CIRCLE ( 'NONE', #11066, 1.875500000000000167 ) ;
#14244 = CARTESIAN_POINT ( 'NONE',  ( 0.6179999999999962190, -1.679378605318048390, 2.054378605318054607 ) ) ;
#14245 = DIRECTION ( 'NONE',  ( 0.000000000000000000, 0.000000000000000000, 1.000000000000000000 ) ) ;
#14246 = CLOSED_SHELL ( 'NONE', ( #7224, #1225, #13351, #3713, #2693, #606, #3042, #3341, #7545, #7459, #6848, #4453, #7537, #5172, #4761, #12412, #14181, #2718, #9551, #7865, #14929, #2968, #9286, #2962, #9657, #324, #11659, #13229, #11812 ) ) ;
#14247 = CARTESIAN_POINT ( 'NONE',  ( 0.6975252985509352577, 0.000000000000000000, 0.000000000000000000 ) ) ;
#14248 = DIRECTION ( 'NONE',  ( 0.000000000000000000, 1.000000000000000000, 0.000000000000000000 ) ) ;
#14249 = EDGE_CURVE ( 'NONE', #6864, #3105, #2181, .T. ) ;
#14250 = CIRCLE ( 'NONE', #13024, 0.03999999999999998002 ) ;
#14251 = ORIENTED_EDGE ( 'NONE', *, *, #10256, .F. ) ;
#14252 = ORIENTED_EDGE ( 'NONE', *, *, #5030, .F. ) ;
#14253 = ORIENTED_EDGE ( 'NONE', *, *, #11972, .F. ) ;
#14254 = CIRCLE ( 'NONE', #10357, 3.000000000000000444 ) ;
#14255 = FACE_OUTER_BOUND ( 'NONE', #12274, .T. ) ;
#14256 = DIRECTION ( 'NONE',  ( -1.000000000000000000, 0.000000000000000000, 0.000000000000000000 ) ) ;
#14257 = CARTESIAN_POINT ( 'NONE',  ( -0.4108223460329323840, 5.750000472440944144, 0.2849999999999956457 ) ) ;
#14258 = LINE ( 'NONE', #9761, #14858 ) ;
#14259 = CARTESIAN_POINT ( 'NONE',  ( 3.760674742763851164, 1.911053679983126141, -0.4872933924078399759 ) ) ;
#14260 = CARTESIAN_POINT ( 'NONE',  ( 1.000000000000000222, -0.4429999999999998939, 0.4258697216429003785 ) ) ;
#14261 = VECTOR ( 'NONE', #11627, 39.37007874015748143 ) ;
#14262 = SURFACE_STYLE_FILL_AREA ( #7329 ) ;
#14263 = EDGE_CURVE ( 'NONE', #14728, #14802, #7248, .T. ) ;
#14264 = AXIS2_PLACEMENT_3D ( 'NONE', #12598, #4661, #8271 ) ;
#14265 = EDGE_CURVE ( 'NONE', #8543, #6823, #2973, .T. ) ;
#14266 = EDGE_CURVE ( 'NONE', #10754, #6601, #812, .T. ) ;
#14267 = DIRECTION ( 'NONE',  ( 0.000000000000000000, 0.000000000000000000, -1.000000000000000000 ) ) ;
#14268 = ORIENTED_EDGE ( 'NONE', *, *, #13509, .F. ) ;
#14270 = ORIENTED_EDGE ( 'NONE', *, *, #13056, .F. ) ;
#14269 = DIRECTION ( 'NONE',  ( 0.000000000000000000, -1.000000000000000000, 0.000000000000000000 ) ) ;
#14271 = EDGE_CURVE ( 'NONE', #5284, #5828, #4712, .T. ) ;
#14272 = VECTOR ( 'NONE', #12418, 39.37007874015748143 ) ;
#14273 = EDGE_LOOP ( 'NONE', ( #5484, #8813, #5378, #14514 ) ) ;
#14274 = CARTESIAN_POINT ( 'NONE',  ( 0.09500000000000431710, -1.679378605318048390, 2.054378605318054607 ) ) ;
#14275 = ORIENTED_EDGE ( 'NONE', *, *, #3266, .T. ) ;
#14276 = DIRECTION ( 'NONE',  ( 1.000000000000000000, 0.000000000000000000, 0.000000000000000000 ) ) ;
#14277 = CARTESIAN_POINT ( 'NONE',  ( 1.569329279054357817, -0.05999999999999986594, -0.4778343322167463159 ) ) ;
#14278 = PRODUCT_CONTEXT ( 'NONE', #13279, 'mechanical' ) ;
#14279 = DIRECTION ( 'NONE',  ( -1.000000000000000000, -0.000000000000000000, -0.000000000000000000 ) ) ;
#14280 = ORIENTED_EDGE ( 'NONE', *, *, #11422, .F. ) ;
#14281 = DIRECTION ( 'NONE',  ( 0.9999002670844989726, 1.365787769249574676E-16, 0.01412288512831212997 ) ) ;
#14282 = CARTESIAN_POINT ( 'NONE',  ( 0.9999999999999996669, 1.557000000000000162, 0.5000000000000000000 ) ) ;
#14283 = CARTESIAN_POINT ( 'NONE',  ( 3.944129661530210385, 0.000000000000000000, 0.000000000000000000 ) ) ;
#14284 = DIRECTION ( 'NONE',  ( 0.000000000000000000, 0.000000000000000000, -1.000000000000000000 ) ) ;
#14285 = CIRCLE ( 'NONE', #7936, 0.7406097974541305806 ) ;
#14286 = DIRECTION ( 'NONE',  ( -0.000000000000000000, -1.000000000000000000, -0.000000000000000000 ) ) ;
#14287 = VECTOR ( 'NONE', #760, 39.37007874015748143 ) ;
#14288 = AXIS2_PLACEMENT_3D ( 'NONE', #8370, #14161, #15083 ) ;
#14289 = CARTESIAN_POINT ( 'NONE',  ( 0.8604590016951504383, -0.4457786592069787335, -0.4394318790773389938 ) ) ;
#14290 = CARTESIAN_POINT ( 'NONE',  ( 3.590089328403619273, 1.905315664284169541, 0.6937522868107603990 ) ) ;
#14291 = DIRECTION ( 'NONE',  ( -1.000000000000000000, -0.000000000000000000, -0.000000000000000000 ) ) ;
#14292 = ORIENTED_EDGE ( 'NONE', *, *, #14819, .T. ) ;
#14293 = FACE_OUTER_BOUND ( 'NONE', #2902, .T. ) ;
#14295 = EDGE_LOOP ( 'NONE', ( #10498, #12568, #10722, #1712 ) ) ;
#14294 = FACE_OUTER_BOUND ( 'NONE', #5748, .T. ) ;
#14296 = ORIENTED_EDGE ( 'NONE', *, *, #5323, .T. ) ;
#14297 = EDGE_CURVE ( 'NONE', #14857, #5088, #1354, .T. ) ;
#14298 = LINE ( 'NONE', #10719, #655 ) ;
#14299 = AXIS2_PLACEMENT_3D ( 'NONE', #13303, #3990, #6219 ) ;
#14300 =( CONVERSION_BASED_UNIT ( 'INCH', #6206 ) LENGTH_UNIT ( ) NAMED_UNIT ( #6287 ) );
#14301 = CARTESIAN_POINT ( 'NONE',  ( 3.112533253352849805, 0.6487563425743173573, 0.3962704070064358985 ) ) ;
#14302 = ORIENTED_EDGE ( 'NONE', *, *, #8407, .F. ) ;
#14303 = CARTESIAN_POINT ( 'NONE',  ( 2.414213562373087374, 0.1427864376268978830, -0.4064941968476759038 ) ) ;
#14304 = CIRCLE ( 'NONE', #9908, 0.3750000000000007772 ) ;
#14305 = VECTOR ( 'NONE', #3832, 39.37007874015748143 ) ;
#14306 = EDGE_CURVE ( 'NONE', #1972, #1062, #9386, .T. ) ;
#14307 = CARTESIAN_POINT ( 'NONE',  ( 0.7073825753665664573, 0.002585322401334269778, 0.4167523536742891443 ) ) ;
#14308 = CARTESIAN_POINT ( 'NONE',  ( 3.426491571325181340, 2.400000000000011458, 0.6999999999999614309 ) ) ;
#14309 = ORIENTED_EDGE ( 'NONE', *, *, #8994, .T. ) ;
#14310 = TOROIDAL_SURFACE ( 'NONE', #6512, 1.580000000000000071, 0.08000000000000000167 ) ;
#14311 = CARTESIAN_POINT ( 'NONE',  ( 6.176491571325181340, -1.679378605318047946, -2.086378605318055968 ) ) ;
#14312 = DIRECTION ( 'NONE',  ( -1.000000000000000000, -0.000000000000000000, -0.000000000000000000 ) ) ;
#14313 = AXIS2_PLACEMENT_3D ( 'NONE', #5778, #9459, #12877 ) ;
#14314 = DIRECTION ( 'NONE',  ( -1.000000000000000000, -0.000000000000000000, -0.000000000000000000 ) ) ;
#14315 = AXIS2_PLACEMENT_3D ( 'NONE', #8362, #1364, #6051 ) ;
#14316 = ORIENTED_EDGE ( 'NONE', *, *, #14457, .F. ) ;
#14317 = DIRECTION ( 'NONE',  ( 0.000000000000000000, 0.000000000000000000, -1.000000000000000000 ) ) ;
#14318 = ORIENTED_EDGE ( 'NONE', *, *, #4476, .T. ) ;
#14319 = CARTESIAN_POINT ( 'NONE',  ( -0.2405759291534545763, 1.577705975193670840, 0.3452157735801421046 ) ) ;
#14320 = ORIENTED_EDGE ( 'NONE', *, *, #1455, .T. ) ;
#14321 = DIRECTION ( 'NONE',  ( -0.000000000000000000, -1.000000000000000000, -0.000000000000000000 ) ) ;
#14322 = EDGE_CURVE ( 'NONE', #6459, #4442, #8226, .T. ) ;
#14323 = ADVANCED_FACE ( 'NONE', ( #92, #15107, #4874, #4791, #9542, #3647 ), #12882, .F. ) ;
#14324 = AXIS2_PLACEMENT_3D ( 'NONE', #5057, #9720, #4046 ) ;
#14325 = CARTESIAN_POINT ( 'NONE',  ( 1.532626322880889402, 0.1749999999999999889, -0.5400755080658653506 ) ) ;
#14326 = CARTESIAN_POINT ( 'NONE',  ( 0.4124999999999997558, -0.6290000000000003366, -0.3725000000000000533 ) ) ;
#14327 = DIRECTION ( 'NONE',  ( 0.000000000000000000, 0.000000000000000000, -1.000000000000000000 ) ) ;
#14328 = CARTESIAN_POINT ( 'NONE',  ( 3.874999999999999556, 3.567999999999999616, 1.320000000000000062 ) ) ;
#14329 = CIRCLE ( 'NONE', #14822, 0.1249999999999999029 ) ;
#14330 = ORIENTED_EDGE ( 'NONE', *, *, #8373, .T. ) ;
#14331 = VERTEX_POINT ( 'NONE', #8164 ) ;
#14332 = VERTEX_POINT ( 'NONE', #9309 ) ;
#14333 = CARTESIAN_POINT ( 'NONE',  ( 8.524379033352612822, 0.9303642257649956671, -0.3795991661955845919 ) ) ;
#14334 = DIRECTION ( 'NONE',  ( 0.000000000000000000, 1.000000000000000000, 0.000000000000000000 ) ) ;
#14335 = AXIS2_PLACEMENT_3D ( 'NONE', #1425, #5892, #3671 ) ;
#14336 = CARTESIAN_POINT ( 'NONE',  ( 1.375000000000000000, 0.000000000000000000, 0.000000000000000000 ) ) ;
#14337 = DIRECTION ( 'NONE',  ( -1.000000000000000000, -0.000000000000000000, -0.000000000000000000 ) ) ;
#14338 = DIRECTION ( 'NONE',  ( 0.000000000000000000, 0.000000000000000000, 1.000000000000000000 ) ) ;
#14339 = AXIS2_PLACEMENT_3D ( 'NONE', #8610, #5235, #1706 ) ;
#14340 = CARTESIAN_POINT ( 'NONE',  ( 1.632672928280226810, 0.0005225660665699846837, 0.4769396479056465243 ) ) ;
#14341 = SURFACE_STYLE_FILL_AREA ( #1841 ) ;
#14342 = VECTOR ( 'NONE', #9337, 39.37007874015748143 ) ;
#14343 = ORIENTED_EDGE ( 'NONE', *, *, #12955, .F. ) ;
#14344 = ORIENTED_EDGE ( 'NONE', *, *, #7591, .T. ) ;
#14345 = ORIENTED_EDGE ( 'NONE', *, *, #1168, .T. ) ;
#14346 = FACE_OUTER_BOUND ( 'NONE', #11535, .T. ) ;
#14347 = ADVANCED_FACE ( 'NONE', ( #14255 ), #13808, .T. ) ;
#14348 = LINE ( 'NONE', #335, #3107 ) ;
#14350 = CONICAL_SURFACE ( 'NONE', #14115, 3.000000000000000444, 0.7853981633974415066 ) ;
#14349 = CARTESIAN_POINT ( 'NONE',  ( -0.1807106342563527812, 1.379999999999999671, 3.262375646219079751E-17 ) ) ;
#14351 = APPLICATION_PROTOCOL_DEFINITION ( 'draft international standard', 'automotive_design', 1998, #3728 ) ;
#14352 = CARTESIAN_POINT ( 'NONE',  ( 3.602264755523620465, 0.9969999999999997753, 0.4491205543005138412 ) ) ;
#14353 = ORIENTED_EDGE ( 'NONE', *, *, #6861, .F. ) ;
#14354 = ADVANCED_FACE ( 'NONE', ( #14184 ), #1176, .F. ) ;
#14355 = DIRECTION ( 'NONE',  ( -1.000000000000000000, -0.000000000000000000, -0.000000000000000000 ) ) ;
#14356 = CYLINDRICAL_SURFACE ( 'NONE', #1675, 2.000000000000000000 ) ;
#14357 = VECTOR ( 'NONE', #1143, 39.37007874015748143 ) ;
#14358 = CARTESIAN_POINT ( 'NONE',  ( 3.426491571325181340, 0.9799999999999438050, -2.360000000000016307 ) ) ;
#14359 = EDGE_CURVE ( 'NONE', #4201, #5214, #1325, .T. ) ;
#14360 = CIRCLE ( 'NONE', #13379, 0.2225000000000001421 ) ;
#14361 = DIRECTION ( 'NONE',  ( -0.000000000000000000, -1.000000000000000000, -0.000000000000000000 ) ) ;
#14362 = LINE ( 'NONE', #14146, #9745 ) ;
#14363 = APPLICATION_CONTEXT ( 'automotive_design' ) ;
#14364 = CARTESIAN_POINT ( 'NONE',  ( 3.705204738311406842, 1.834542981759929470, 0.7866137051850492501 ) ) ;
#14365 = DIRECTION ( 'NONE',  ( 0.000000000000000000, 0.000000000000000000, -1.000000000000000000 ) ) ;
#14366 = EDGE_LOOP ( 'NONE', ( #9879, #868, #10096, #14227 ) ) ;
#14367 = DIRECTION ( 'NONE',  ( 0.000000000000000000, 0.000000000000000000, -1.000000000000000000 ) ) ;
#14369 = ORIENTED_EDGE ( 'NONE', *, *, #805, .T. ) ;
#14368 = CARTESIAN_POINT ( 'NONE',  ( 3.875000000000000000, 3.085321731235734610, 0.000000000000000000 ) ) ;
#14370 = CIRCLE ( 'NONE', #13387, 0.8000000000000000444 ) ;
#14371 = VERTEX_POINT ( 'NONE', #10678 ) ;
#14372 = ADVANCED_FACE ( 'NONE', ( #7245 ), #853, .F. ) ;
#14373 = AXIS2_PLACEMENT_3D ( 'NONE', #8200, #13909, #9345 ) ;
#14374 = DIRECTION ( 'NONE',  ( 0.000000000000000000, 1.000000000000000000, 0.000000000000000000 ) ) ;
#14375 = CARTESIAN_POINT ( 'NONE',  ( 2.326828918379972104E-17, 0.03800000000000004763, 0.1900000000000000577 ) ) ;
#14376 = ORIENTED_EDGE ( 'NONE', *, *, #6154, .F. ) ;
#14377 = EDGE_CURVE ( 'NONE', #1005, #1733, #7060, .T. ) ;
#14378 = AXIS2_PLACEMENT_3D ( 'NONE', #12783, #7076, #14006 ) ;
#14379 = DIRECTION ( 'NONE',  ( 0.000000000000000000, 0.000000000000000000, -1.000000000000000000 ) ) ;
#14380 = VECTOR ( 'NONE', #5964, 39.37007874015748143 ) ;
#14381 = CIRCLE ( 'NONE', #7546, 2.967999999999998639 ) ;
#14382 = DIMENSIONAL_EXPONENTS ( 1.000000000000000000, 0.000000000000000000, 0.000000000000000000, 0.000000000000000000, 0.000000000000000000, 0.000000000000000000, 0.000000000000000000 ) ;
#14383 = EDGE_CURVE ( 'NONE', #6823, #3261, #373, .T. ) ;
#14384 = DIRECTION ( 'NONE',  ( -0.000000000000000000, -1.000000000000000000, -0.000000000000000000 ) ) ;
#14385 = CIRCLE ( 'NONE', #9997, 0.6700292969071727223 ) ;
#14386 = FACE_OUTER_BOUND ( 'NONE', #5853, .T. ) ;
#14387 = EDGE_CURVE ( 'NONE', #11436, #2425, #10893, .T. ) ;
#14388 = EDGE_LOOP ( 'NONE', ( #14624, #1927, #8002, #10620 ) ) ;
#14389 = AXIS2_PLACEMENT_3D ( 'NONE', #1022, #12575, #11290 ) ;
#14390 = DIRECTION ( 'NONE',  ( 0.000000000000000000, 0.000000000000000000, -1.000000000000000000 ) ) ;
#14391 = DIRECTION ( 'NONE',  ( -0.000000000000000000, -0.000000000000000000, 1.000000000000000000 ) ) ;
#14392 = LINE ( 'NONE', #3925, #3881 ) ;
#14393 = ORIENTED_EDGE ( 'NONE', *, *, #6538, .T. ) ;
#14394 = AXIS2_PLACEMENT_3D ( 'NONE', #12737, #13726, #3262 ) ;
#14395 = ADVANCED_FACE ( 'NONE', ( #5019 ), #313, .F. ) ;
#14396 = DIRECTION ( 'NONE',  ( 0.000000000000000000, 0.000000000000000000, -1.000000000000000000 ) ) ;
#14397 = ORIENTED_EDGE ( 'NONE', *, *, #3401, .T. ) ;
#14398 = CARTESIAN_POINT ( 'NONE',  ( 0.7095752389709886199, -0.01561891520650799531, 0.4705416541824799515 ) ) ;
#14399 = VERTEX_POINT ( 'NONE', #8753 ) ;
#14400 = SURFACE_SIDE_STYLE ('',( #9742 ) ) ;
#14401 = CIRCLE ( 'NONE', #9993, 0.8083085967350902568 ) ;
#14402 = CARTESIAN_POINT ( 'NONE',  ( 3.426491571325181340, 1.679378605318059048, 1.941878605318041462 ) ) ;
#14403 = ADVANCED_FACE ( 'NONE', ( #1704 ), #12194, .T. ) ;
#14404 = AXIS2_PLACEMENT_3D ( 'NONE', #10138, #934, #4404 ) ;
#14405 = DIRECTION ( 'NONE',  ( 0.9999002670844989726, -2.602203049398214110E-17, 0.01412288512831212997 ) ) ;
#14406 = CARTESIAN_POINT ( 'NONE',  ( 6.208491571325183145, 1.679378605318059492, 1.679378605318041506 ) ) ;
#14407 = DIRECTION ( 'NONE',  ( -1.000000000000000000, -0.000000000000000000, -0.000000000000000000 ) ) ;
#14408 = CARTESIAN_POINT ( 'NONE',  ( 1.993930392107171823, 0.2778841324403868995, -0.4718371413552246429 ) ) ;
#14409 = EDGE_CURVE ( 'NONE', #9027, #8887, #5775, .T. ) ;
#14410 = FACE_OUTER_BOUND ( 'NONE', #13335, .T. ) ;
#14411 = ORIENTED_EDGE ( 'NONE', *, *, #7394, .F. ) ;
#14412 = ORIENTED_EDGE ( 'NONE', *, *, #78, .F. ) ;
#14413 = ORIENTED_EDGE ( 'NONE', *, *, #13412, .T. ) ;
#14414 = AXIS2_PLACEMENT_3D ( 'NONE', #269, #13055, #5965 ) ;
#14415 = DIRECTION ( 'NONE',  ( -0.7071067811865414665, 0.000000000000000000, 0.7071067811865534569 ) ) ;
#14416 = CARTESIAN_POINT ( 'NONE',  ( 0.000000000000000000, 0.000000000000000000, 0.000000000000000000 ) ) ;
#14417 = DIRECTION ( 'NONE',  ( 0.000000000000000000, 0.000000000000000000, -1.000000000000000000 ) ) ;
#14418 = CARTESIAN_POINT ( 'NONE',  ( -5.764454660286586870E-18, -0.2214999999999999469, 0.000000000000000000 ) ) ;
#14419 = CARTESIAN_POINT ( 'NONE',  ( 3.426491571325181340, 1.964030041192035947, -0.6624825471404702792 ) ) ;
#14420 = DIRECTION ( 'NONE',  ( 0.000000000000000000, -1.000000000000000000, 4.591341165822195764E-16 ) ) ;
#14421 = ADVANCED_FACE ( 'NONE', ( #469 ), #4663, .T. ) ;
#14422 = ORIENTED_EDGE ( 'NONE', *, *, #7389, .F. ) ;
#14423 = ORIENTED_EDGE ( 'NONE', *, *, #10014, .F. ) ;
#14424 = ORIENTED_EDGE ( 'NONE', *, *, #6818, .T. ) ;
#14425 = VECTOR ( 'NONE', #10013, 39.37007874015748143 ) ;
#14426 = DIRECTION ( 'NONE',  ( 0.000000000000000000, 0.000000000000000000, 1.000000000000000000 ) ) ;
#14427 = DIRECTION ( 'NONE',  ( -1.000000000000000000, 0.000000000000000000, -9.106159978880873451E-16 ) ) ;
#14428 = DIRECTION ( 'NONE',  ( 0.000000000000000000, 0.000000000000000000, -1.000000000000000000 ) ) ;
#14429 = SHAPE_DEFINITION_REPRESENTATION ( #7626, #10912 ) ;
#14430 = CARTESIAN_POINT ( 'NONE',  ( 6.826491571325181695, 1.679378605318035733, -2.086378605318067958 ) ) ;
#14431 = EDGE_LOOP ( 'NONE', ( #6552, #5575, #9504, #7187, #1804 ) ) ;
#14432 = CARTESIAN_POINT ( 'NONE',  ( 2.124999999999999556, -3.360000000000016751, -0.9799999999999434719 ) ) ;
#14433 = CARTESIAN_POINT ( 'NONE',  ( 2.124999999999999556, -1.679378605318041950, 1.384878605318059064 ) ) ;
#14434 = DIRECTION ( 'NONE',  ( 0.000000000000000000, 1.000000000000000000, 0.000000000000000000 ) ) ;
#14435 = VECTOR ( 'NONE', #4852, 39.37007874015748143 ) ;
#14436 = CARTESIAN_POINT ( 'NONE',  ( 2.774999999999999911, -1.575000000000027489, -2.359999999999989218 ) ) ;
#14437 = CARTESIAN_POINT ( 'NONE',  ( 2.124999999999999556, 1.679378605318059048, 1.679378605318041506 ) ) ;
#14438 = LINE ( 'NONE', #7489, #6877 ) ;
#14439 = CARTESIAN_POINT ( 'NONE',  ( 3.816981501931459242, 1.796899953488545698, 0.7979432928147958126 ) ) ;
#14440 = CARTESIAN_POINT ( 'NONE',  ( 3.426491571325181340, 2.400000000000011458, 0.6999999999999614309 ) ) ;
#14441 = VERTEX_POINT ( 'NONE', #13107 ) ;
#14442 = CARTESIAN_POINT ( 'NONE',  ( 3.394491571325182644, 1.679378605318042395, -1.416878605318058870 ) ) ;
#14444 = ORIENTED_EDGE ( 'NONE', *, *, #13709, .T. ) ;
#14443 = LINE ( 'NONE', #12297, #15058 ) ;
#14445 = ORIENTED_EDGE ( 'NONE', *, *, #8154, .F. ) ;
#14446 = DIRECTION ( 'NONE',  ( -0.7071067811865604513, 0.7071067811865345831, 1.170732267570242325E-16 ) ) ;
#14447 = CARTESIAN_POINT ( 'NONE',  ( 8.475037399843312613, 0.9289129992088659415, 0.3802960819231170908 ) ) ;
#14448 = ORIENTED_EDGE ( 'NONE', *, *, #7106, .T. ) ;
#14449 = AXIS2_PLACEMENT_3D ( 'NONE', #2421, #12885, #8332 ) ;
#14450 = DIRECTION ( 'NONE',  ( 0.000000000000000000, 0.000000000000000000, 1.000000000000000000 ) ) ;
#14451 = LINE ( 'NONE', #10031, #3143 ) ;
#14452 = CARTESIAN_POINT ( 'NONE',  ( 0.6552631510457654906, -0.03278499996209151279, 0.5075199847260384312 ) ) ;
#14453 = EDGE_CURVE ( 'NONE', #9247, #6889, #2643, .T. ) ;
#14454 = CARTESIAN_POINT ( 'NONE',  ( 2.124999999999999556, -1.574999999999984190, 1.575000000000033040 ) ) ;
#14455 = EDGE_CURVE ( 'NONE', #4088, #14179, #8546, .T. ) ;
#14456 = ORIENTED_EDGE ( 'NONE', *, *, #6452, .T. ) ;
#14457 = EDGE_CURVE ( 'NONE', #863, #12982, #11375, .T. ) ;
#14458 = DIRECTION ( 'NONE',  ( 1.000000000000000000, 0.000000000000000000, 0.000000000000000000 ) ) ;
#14459 = CARTESIAN_POINT ( 'NONE',  ( -0.4124999999999999223, 0.1749999999999999889, -0.4124999999999999778 ) ) ;
#14460 = DIRECTION ( 'NONE',  ( -0.7070715176384863021, -0.7070715176384774203, -0.009986885842351498482 ) ) ;
#14461 = DIRECTION ( 'NONE',  ( 0.000000000000000000, 0.000000000000000000, 1.000000000000000000 ) ) ;
#14462 = VERTEX_POINT ( 'NONE', #12116 ) ;
#14463 = EDGE_CURVE ( 'NONE', #12577, #34, #10900, .T. ) ;
#14464 = CARTESIAN_POINT ( 'NONE',  ( 0.7034553201775792797, -0.02513445208134620565, 0.4790822413290390935 ) ) ;
#14465 = ORIENTED_EDGE ( 'NONE', *, *, #4750, .T. ) ;
#14466 = DIRECTION ( 'NONE',  ( 1.000000000000000000, 0.000000000000000000, 0.000000000000000000 ) ) ;
#14467 = AXIS2_PLACEMENT_3D ( 'NONE', #7075, #3700, #11736 ) ;
#14468 = DIRECTION ( 'NONE',  ( 1.000000000000000000, 0.000000000000000000, 0.000000000000000000 ) ) ;
#14469 = CARTESIAN_POINT ( 'NONE',  ( 0.8254245316410399047, -0.4829999999999998739, -0.3670313414528084683 ) ) ;
#14470 = DIRECTION ( 'NONE',  ( -0.7071067811865421326, 0.000000000000000000, 0.7071067811865527908 ) ) ;
#14471 = CARTESIAN_POINT ( 'NONE',  ( 0.000000000000000000, 5.750000000000000000, 0.000000000000000000 ) ) ;
#14472 = CARTESIAN_POINT ( 'NONE',  ( 2.045923089166570730, 0.3299328314968389964, -0.4711027812264609871 ) ) ;
#14473 = AXIS2_PLACEMENT_3D ( 'NONE', #8019, #4423, #3495 ) ;
#14474 = ORIENTED_EDGE ( 'NONE', *, *, #12097, .F. ) ;
#14475 = ORIENTED_EDGE ( 'NONE', *, *, #4381, .T. ) ;
#14476 = ORIENTED_EDGE ( 'NONE', *, *, #4401, .F. ) ;
#14477 = DIRECTION ( 'NONE',  ( 0.000000000000000000, 0.000000000000000000, -1.000000000000000000 ) ) ;
#14478 = AXIS2_PLACEMENT_3D ( 'NONE', #185, #8102, #13811 ) ;
#14479 = PLANE ( 'NONE',  #13596 ) ;
#14480 = ADVANCED_FACE ( 'NONE', ( #7458 ), #10660, .F. ) ;
#14481 = DIRECTION ( 'NONE',  ( -0.000000000000000000, -1.000000000000000000, -0.000000000000000000 ) ) ;
#14482 = CARTESIAN_POINT ( 'NONE',  ( 2.774999999999999911, 1.575000000000016609, 1.575000000000000178 ) ) ;
#14483 = DIRECTION ( 'NONE',  ( 0.000000000000000000, 0.000000000000000000, -1.000000000000000000 ) ) ;
#14484 = ADVANCED_FACE ( 'NONE', ( #7833 ), #6017, .T. ) ;
#14485 = CARTESIAN_POINT ( 'NONE',  ( 4.525161324076911740, 1.792777560986625662, 0.3773916261770783320 ) ) ;
#14486 = AXIS2_PLACEMENT_3D ( 'NONE', #9266, #3514, #2285 ) ;
#14487 = AXIS2_PLACEMENT_3D ( 'NONE', #3549, #7001, #9215 ) ;
#14488 = ORIENTED_EDGE ( 'NONE', *, *, #1396, .F. ) ;
#14489 = EDGE_LOOP ( 'NONE', ( #5220, #5242, #5153, #6803 ) ) ;
#14490 = ORIENTED_EDGE ( 'NONE', *, *, #10382, .T. ) ;
#14491 = DIRECTION ( 'NONE',  ( 0.000000000000000000, 0.000000000000000000, -1.000000000000000000 ) ) ;
#14492 = FACE_OUTER_BOUND ( 'NONE', #1445, .T. ) ;
#14493 = CARTESIAN_POINT ( 'NONE',  ( 4.298771110290672048, 0.9641137807165872653, 0.2658577392121701521 ) ) ;
#14494 = DIRECTION ( 'NONE',  ( 0.000000000000000000, 1.000000000000000000, -4.591341165822195764E-16 ) ) ;
#14495 = ORIENTED_EDGE ( 'NONE', *, *, #14833, .F. ) ;
#14496 = CIRCLE ( 'NONE', #4745, 0.2944999999999856066 ) ;
#14497 = DIRECTION ( 'NONE',  ( 0.000000000000000000, 0.000000000000000000, -1.000000000000000000 ) ) ;
#14498 = CARTESIAN_POINT ( 'NONE',  ( 2.527624975756972425, 3.137999999999999901, -0.9199802545633498640 ) ) ;
#14499 = CIRCLE ( 'NONE', #15004, 1.000000000000000222 ) ;
#14500 = ADVANCED_FACE ( 'NONE', ( #3013 ), #845, .F. ) ;
#14501 = EDGE_CURVE ( 'NONE', #3716, #11155, #12586, .T. ) ;
#14502 = DIRECTION ( 'NONE',  ( 0.000000000000000000, 0.000000000000000000, -1.000000000000000000 ) ) ;
#14503 = CARTESIAN_POINT ( 'NONE',  ( 3.426491571325181340, 0.9799999999999436939, -3.360000000000016751 ) ) ;
#14504 = FACE_OUTER_BOUND ( 'NONE', #11935, .T. ) ;
#14505 = CIRCLE ( 'NONE', #8669, 0.2944999999999979301 ) ;
#14506 = AXIS2_PLACEMENT_3D ( 'NONE', #7278, #1441, #6130 ) ;
#14507 = CARTESIAN_POINT ( 'NONE',  ( 2.124999999999999556, 1.679378605318059048, 1.973878605318041268 ) ) ;
#14509 = EDGE_LOOP ( 'NONE', ( #3831, #1609, #3209, #11589 ) ) ;
#14508 = CARTESIAN_POINT ( 'NONE',  ( 0.000000000000000000, 0.000000000000000000, 0.2041999999999996596 ) ) ;
#14510 = ORIENTED_EDGE ( 'NONE', *, *, #831, .T. ) ;
#14511 = DIRECTION ( 'NONE',  ( -1.000000000000000000, -0.000000000000000000, -0.000000000000000000 ) ) ;
#14513 = ORIENTED_EDGE ( 'NONE', *, *, #5302, .F. ) ;
#14512 = DIRECTION ( 'NONE',  ( 0.000000000000000000, -1.000000000000000000, 0.000000000000000000 ) ) ;
#14514 = ORIENTED_EDGE ( 'NONE', *, *, #4316, .F. ) ;
#14515 = DIRECTION ( 'NONE',  ( -0.5000000000000000000, 0.000000000000000000, 0.8660254037844385966 ) ) ;
#14516 =( NAMED_UNIT ( * ) SI_UNIT ( $, .STERADIAN. ) SOLID_ANGLE_UNIT ( ) );
#14517 = LINE ( 'NONE', #11012, #13771 ) ;
#14518 = ORIENTED_EDGE ( 'NONE', *, *, #1824, .F. ) ;
#14519 = DIRECTION ( 'NONE',  ( 0.000000000000000000, 0.000000000000000000, -1.000000000000000000 ) ) ;
#14520 = CARTESIAN_POINT ( 'NONE',  ( 0.000000000000000000, 0.03800000000000004763, 0.000000000000000000 ) ) ;
#14521 = VECTOR ( 'NONE', #11118, 39.37007874015748143 ) ;
#14522 = EDGE_CURVE ( 'NONE', #12064, #5075, #7485, .T. ) ;
#14523 = AXIS2_PLACEMENT_3D ( 'NONE', #8461, #7316, #13100 ) ;
#14524 = AXIS2_PLACEMENT_3D ( 'NONE', #4365, #14757, #14835 ) ;
#14525 = CARTESIAN_POINT ( 'NONE',  ( 0.7013471289190064129, -0.03216119633915270892, 0.4834044059207765476 ) ) ;
#14526 = CARTESIAN_POINT ( 'NONE',  ( 0.4425000000000001155, 0.2159999999999999420, -0.8500000000000000888 ) ) ;
#14527 = VERTEX_POINT ( 'NONE', #11273 ) ;
#14528 = LINE ( 'NONE', #14235, #8049 ) ;
#14529 = CARTESIAN_POINT ( 'NONE',  ( 3.875000000000000000, 3.535499999999999865, 0.4849999999999995981 ) ) ;
#14530 = DIRECTION ( 'NONE',  ( 0.000000000000000000, 1.000000000000000000, 0.000000000000000000 ) ) ;
#14531 = VECTOR ( 'NONE', #14600, 39.37007874015748854 ) ;
#14532 = LINE ( 'NONE', #2221, #10406 ) ;
#14533 = CARTESIAN_POINT ( 'NONE',  ( 3.426491571325181340, 1.574999999999994849, -1.575000000000022160 ) ) ;
#14534 = VERTEX_POINT ( 'NONE', #13776 ) ;
#14535 = VECTOR ( 'NONE', #10746, 39.37007874015748143 ) ;
#14536 = VECTOR ( 'NONE', #14066, 39.37007874015748143 ) ;
#14537 = DIRECTION ( 'NONE',  ( -1.000000000000000000, 0.000000000000000000, 0.000000000000000000 ) ) ;
#14538 = EDGE_LOOP ( 'NONE', ( #6551, #11193, #13718, #1118, #9792, #3834, #12232, #12712, #13128, #7990 ) ) ;
#14539 = EDGE_CURVE ( 'NONE', #9198, #4559, #6618, .T. ) ;
#14540 = LENGTH_MEASURE_WITH_UNIT ( LENGTH_MEASURE( 0.02539999999999999897 ), #6521 );
#14541 = EDGE_CURVE ( 'NONE', #3175, #5637, #8237, .T. ) ;
#14542 = EDGE_CURVE ( 'NONE', #5828, #8206, #2094, .T. ) ;
#14543 = DIRECTION ( 'NONE',  ( -1.000000000000000000, -0.000000000000000000, -0.000000000000000000 ) ) ;
#14544 = VECTOR ( 'NONE', #2395, 39.37007874015748854 ) ;
#14545 = CARTESIAN_POINT ( 'NONE',  ( 1.131687341751771880, -0.4429445645322995784, 0.4840157155121827537 ) ) ;
#14546 = CARTESIAN_POINT ( 'NONE',  ( 0.8395363466603752434, -0.4830000013348689780, -0.3304764024893170338 ) ) ;
#14547 = DIRECTION ( 'NONE',  ( 0.000000000000000000, 0.000000000000000000, -1.000000000000000000 ) ) ;
#14548 = VECTOR ( 'NONE', #13861, 39.37007874015748143 ) ;
#14549 = AXIS2_PLACEMENT_3D ( 'NONE', #10133, #3239, #4172 ) ;
#14550 = EDGE_CURVE ( 'NONE', #4931, #8434, #1605, .T. ) ;
#14551 = B_SPLINE_CURVE_WITH_KNOTS ( 'NONE', 3,
 ( #11322, #980, #9111, #8050, #3152, #12535, #5671, #4445, #5599, #4296, #11251, #10039 ),
 .UNSPECIFIED., .F., .F.,
 ( 4, 2, 2, 2, 2, 4 ),
 ( 0.000000000000000000, 0.003650815867420974421, 0.007301631734841948843, 0.009127039668552414803, 0.01095244760226288423, 0.01460326346968381268 ),
 .UNSPECIFIED. ) ;
#14552 = DIRECTION ( 'NONE',  ( 0.000000000000000000, -0.000000000000000000, 1.000000000000000000 ) ) ;
#14553 = CARTESIAN_POINT ( 'NONE',  ( 1.973685276483752471, 0.1827974636779304551, -0.4721230893152013053 ) ) ;
#14554 = CARTESIAN_POINT ( 'NONE',  ( 3.874999999999999556, 2.750000000000000000, -1.098000000000000087 ) ) ;
#14555 = ORIENTED_EDGE ( 'NONE', *, *, #1108, .T. ) ;
#14556 = EDGE_LOOP ( 'NONE', ( #6012, #6093 ) ) ;
#14557 = VERTEX_POINT ( 'NONE', #12338 ) ;
#14558 = VECTOR ( 'NONE', #11486, 39.37007874015748143 ) ;
#14559 = DIRECTION ( 'NONE',  ( -1.000000000000000000, 0.000000000000000000, -0.000000000000000000 ) ) ;
#14560 = ORIENTED_EDGE ( 'NONE', *, *, #3207, .T. ) ;
#14561 = DIRECTION ( 'NONE',  ( 0.000000000000000000, 0.000000000000000000, -1.000000000000000000 ) ) ;
#14562 = EDGE_CURVE ( 'NONE', #11419, #8572, #8703, .T. ) ;
#14563 = DIRECTION ( 'NONE',  ( 1.000000000000000000, 0.000000000000000000, 0.000000000000000000 ) ) ;
#14564 = CARTESIAN_POINT ( 'NONE',  ( 4.368012994362165280, 1.779897144447762702, 0.5670951116580714713 ) ) ;
#14565 = ADVANCED_BREP_SHAPE_REPRESENTATION ( '', ( #10641, #8424 ), #7206 ) ;
#14566 = CONICAL_SURFACE ( 'NONE', #11645, 0.3750000000000004996, 0.7853981633974536081 ) ;
#14567 = EDGE_CURVE ( 'NONE', #9809, #6905, #6809, .T. ) ;
#14568 = AXIS2_PLACEMENT_3D ( 'NONE', #6335, #5039, #554 ) ;
#14569 = CARTESIAN_POINT ( 'NONE',  ( 4.042576247476339368, 1.760009672272428993, -0.7323577104505313295 ) ) ;
#14570 = EDGE_LOOP ( 'NONE', ( #12633, #11805, #9228, #6909 ) ) ;
#14571 = VERTEX_POINT ( 'NONE', #3176 ) ;
#14572 = EDGE_CURVE ( 'NONE', #4719, #14941, #698, .T. ) ;
#14573 = EDGE_LOOP ( 'NONE', ( #478, #12160, #4962, #13317 ) ) ;
#14574 = CARTESIAN_POINT ( 'NONE',  ( 0.2099999999999999922, 1.559103846021539619, 0.3809527529760087239 ) ) ;
#14575 = CARTESIAN_POINT ( 'NONE',  ( 0.8999999999999998002, 0.01999999999999975409, -0.3799999999999999489 ) ) ;
#14576 = CARTESIAN_POINT ( 'NONE',  ( 4.348909005209756984, 0.9871496092524738586, -0.1627569400240113373 ) ) ;
#14577 = ITEM_DEFINED_TRANSFORMATION ( 'NONE', 'NONE', #11833,  #8424 ) ;
#14578 = CARTESIAN_POINT ( 'NONE',  ( 3.099256572624754735, 0.9349522984520411972, 0.4562251896521927197 ) ) ;
#14579 = ORIENTED_EDGE ( 'NONE', *, *, #7198, .F. ) ;
#14580 =( BOUNDED_CURVE ( )  B_SPLINE_CURVE ( 3, ( #397, #543, #9829, #2945 ),
 .UNSPECIFIED., .F., .F. ) 
 B_SPLINE_CURVE_WITH_KNOTS ( ( 4, 4 ),
 ( 0.000000000000000000, 1.556672972142350675 ),
 .UNSPECIFIED. ) 
 CURVE ( )  GEOMETRIC_REPRESENTATION_ITEM ( )  RATIONAL_B_SPLINE_CURVE ( ( 1.000000000000000000, 0.8080549792898082950, 0.8080549792898082950, 1.000000000000000000 ) ) 
 REPRESENTATION_ITEM ( '' )  );
#14581 = CARTESIAN_POINT ( 'NONE',  ( 0.000000000000000000, 0.000000000000000000, 0.000000000000000000 ) ) ;
#14582 = DIRECTION ( 'NONE',  ( 0.01412288512831583534, 0.000000000000000000, 0.9999002670844989726 ) ) ;
#14583 = CARTESIAN_POINT ( 'NONE',  ( 3.426491571325181340, -2.360000000000016751, -0.9799999999999431388 ) ) ;
#14584 = FACE_OUTER_BOUND ( 'NONE', #2552, .T. ) ;
#14585 = CARTESIAN_POINT ( 'NONE',  ( 6.826491571325181695, 0.000000000000000000, 0.000000000000000000 ) ) ;
#14586 = FACE_OUTER_BOUND ( 'NONE', #14863, .T. ) ;
#14587 = DIRECTION ( 'NONE',  ( -1.000000000000000000, -0.000000000000000000, -0.000000000000000000 ) ) ;
#14588 = CARTESIAN_POINT ( 'NONE',  ( 4.487514378271046489, 1.732936262643785419, 0.4354029880432472299 ) ) ;
#14590 = VERTEX_POINT ( 'NONE', #3095 ) ;
#14589 = CARTESIAN_POINT ( 'NONE',  ( 3.426491571325181340, 2.359999999999994547, -1.575000000000016831 ) ) ;
#14591 = EDGE_CURVE ( 'NONE', #7643, #2188, #3579, .T. ) ;
#14592 = EDGE_CURVE ( 'NONE', #11914, #13586, #9457, .T. ) ;
#14593 = ORIENTED_EDGE ( 'NONE', *, *, #6076, .F. ) ;
#14594 = CARTESIAN_POINT ( 'NONE',  ( -0.2249147617188422821, 1.559103846021539619, -0.3723417112827360209 ) ) ;
#14596 = VERTEX_POINT ( 'NONE', #11425 ) ;
#14595 = DIRECTION ( 'NONE',  ( 0.000000000000000000, 0.000000000000000000, 1.000000000000000000 ) ) ;
#14597 = ORIENTED_EDGE ( 'NONE', *, *, #4997, .F. ) ;
#14598 = CIRCLE ( 'NONE', #4099, 0.3750000000000004996 ) ;
#14599 = CARTESIAN_POINT ( 'NONE',  ( 3.944129661530210385, 1.761538328845252188, -0.7935532608319411096 ) ) ;
#14600 = DIRECTION ( 'NONE',  ( -0.9999002670844989726, -1.365787769249574676E-16, -0.01412288512831212997 ) ) ;
#14601 = ORIENTED_EDGE ( 'NONE', *, *, #5682, .T. ) ;
#14602 = CARTESIAN_POINT ( 'NONE',  ( 0.3725000000000000533, 0.000000000000000000, -0.3724999999999999978 ) ) ;
#14603 = DIRECTION ( 'NONE',  ( 0.000000000000000000, 1.000000000000000000, 0.000000000000000000 ) ) ;
#14604 = DIRECTION ( 'NONE',  ( 0.000000000000000000, 1.000000000000000000, 0.000000000000000000 ) ) ;
#14605 = VECTOR ( 'NONE', #13269, 39.37007874015748143 ) ;
#14606 = AXIS2_PLACEMENT_3D ( 'NONE', #13022, #4705, #11816 ) ;
#14607 = CARTESIAN_POINT ( 'NONE',  ( 0.7026404547606494022, -0.05184959461285652826, 0.4896627279036661617 ) ) ;
#14608 = CARTESIAN_POINT ( 'NONE',  ( 0.3724999999999997757, -0.6290000000000004476, -0.4125000000000000333 ) ) ;
#14609 = ORIENTED_EDGE ( 'NONE', *, *, #14377, .F. ) ;
#14610 = DIRECTION ( 'NONE',  ( -0.000000000000000000, -1.000000000000000000, -0.000000000000000000 ) ) ;
#14611 = AXIS2_PLACEMENT_3D ( 'NONE', #10050, #9125, #11107 ) ;
#14612 = DIRECTION ( 'NONE',  ( -0.3420201433256623846, 0.000000000000000000, 0.9396926207859106484 ) ) ;
#14613 = AXIS2_PLACEMENT_3D ( 'NONE', #14406, #9890, #14547 ) ;
#14614 = DIRECTION ( 'NONE',  ( 2.602462600580851747E-17, 1.000000000000000000, -0.000000000000000000 ) ) ;
#14615 = ORIENTED_EDGE ( 'NONE', *, *, #10727, .F. ) ;
#14616 = VECTOR ( 'NONE', #11477, 39.37007874015748143 ) ;
#14617 = EDGE_CURVE ( 'NONE', #4263, #6919, #861, .T. ) ;
#14618 = CIRCLE ( 'NONE', #663, 0.1899999999999996136 ) ;
#14619 = CARTESIAN_POINT ( 'NONE',  ( 6.215861650065340527, 0.000000000000000000, -3.000000000000000444 ) ) ;
#14620 = CARTESIAN_POINT ( 'NONE',  ( 3.876560711617219379, 3.567999999999999616, 0.000000000000000000 ) ) ;
#14621 = ORIENTED_EDGE ( 'NONE', *, *, #8963, .F. ) ;
#14622 = AXIS2_PLACEMENT_3D ( 'NONE', #811, #1814, #8722 ) ;
#14623 = CYLINDRICAL_SURFACE ( 'NONE', #2282, 1.500000000000000222 ) ;
#14624 = ORIENTED_EDGE ( 'NONE', *, *, #7455, .F. ) ;
#14625 =( CONVERSION_BASED_UNIT ( 'INCH', #14540 ) LENGTH_UNIT ( ) NAMED_UNIT ( #4141 ) );
#14626 = AXIS2_PLACEMENT_3D ( 'NONE', #7878, #12310, #5513 ) ;
#14627 = CARTESIAN_POINT ( 'NONE',  ( 4.344846310392954436, 3.137999999999999901, -1.491010071662831171 ) ) ;
#14628 = AXIS2_PLACEMENT_3D ( 'NONE', #9592, #13300, #5071 ) ;
#14629 = CARTESIAN_POINT ( 'NONE',  ( 0.000000000000000000, -1.002374524060224757E-18, 0.1520000000000001905 ) ) ;
#14630 = CONICAL_SURFACE ( 'NONE', #1434, 0.3750000000000004996, 0.7853981633974503884 ) ;
#14631 = DIRECTION ( 'NONE',  ( 0.000000000000000000, 0.000000000000000000, 1.000000000000000000 ) ) ;
#14632 = VECTOR ( 'NONE', #3035, 39.37007874015748143 ) ;
#14633 = ORIENTED_EDGE ( 'NONE', *, *, #364, .T. ) ;
#14634 = AXIS2_PLACEMENT_3D ( 'NONE', #13275, #3120, #12363 ) ;
#14635 = CARTESIAN_POINT ( 'NONE',  ( 0.000000000000000000, 0.000000000000000000, 0.000000000000000000 ) ) ;
#14636 = EDGE_CURVE ( 'NONE', #4088, #9247, #5534, .T. ) ;
#14637 = CARTESIAN_POINT ( 'NONE',  ( 1.612492615670229279, 0.05745813234176332107, -0.4169456318805929707 ) ) ;
#14638 = PRESENTATION_STYLE_ASSIGNMENT (( #13399 ) ) ;
#14639 = CARTESIAN_POINT ( 'NONE',  ( 0.06299999999999998657, 0.000000000000000000, 0.000000000000000000 ) ) ;
#14640 = ORIENTED_EDGE ( 'NONE', *, *, #2162, .F. ) ;
#14641 = ORIENTED_EDGE ( 'NONE', *, *, #9530, .F. ) ;
#14642 = VERTEX_POINT ( 'NONE', #1004 ) ;
#14643 = CARTESIAN_POINT ( 'NONE',  ( 3.875000000000000000, 3.085321731235734610, -0.4849999999999995981 ) ) ;
#14644 = VERTEX_POINT ( 'NONE', #14643 ) ;
#14645 = DIRECTION ( 'NONE',  ( 0.000000000000000000, 0.000000000000000000, -1.000000000000000000 ) ) ;
#14646 = CARTESIAN_POINT ( 'NONE',  ( 3.906623289280057325E-17, 0.000000000000000000, 0.3190000000000000058 ) ) ;
#14647 = AXIS2_PLACEMENT_3D ( 'NONE', #9469, #11903, #3574 ) ;
#14648 = DIRECTION ( 'NONE',  ( -1.000000000000000000, -0.000000000000000000, -0.000000000000000000 ) ) ;
#14649 = DIRECTION ( 'NONE',  ( 0.000000000000000000, 0.000000000000000000, -1.000000000000000000 ) ) ;
#14650 = ORIENTED_EDGE ( 'NONE', *, *, #8325, .F. ) ;
#14651 = ADVANCED_FACE ( 'NONE', ( #8834 ), #14071, .T. ) ;
#14652 = AXIS2_PLACEMENT_3D ( 'NONE', #2324, #13939, #12793 ) ;
#14653 = EDGE_CURVE ( 'NONE', #7301, #7227, #13551, .T. ) ;
#14654 = EDGE_CURVE ( 'NONE', #3585, #5441, #135, .T. ) ;
#14655 = VERTEX_POINT ( 'NONE', #7231 ) ;
#14656 = VERTEX_POINT ( 'NONE', #1159 ) ;
#14657 = VERTEX_POINT ( 'NONE', #5925 ) ;
#14658 = CARTESIAN_POINT ( 'NONE',  ( 0.2405759291534288191, 1.577705975193649968, -0.3452157735801837934 ) ) ;
#14659 = DIRECTION ( 'NONE',  ( 0.000000000000000000, 0.000000000000000000, -1.000000000000000000 ) ) ;
#14660 = CARTESIAN_POINT ( 'NONE',  ( 2.743000000000000327, 1.679378605318042395, -1.679378605318058604 ) ) ;
#14661 = EDGE_CURVE ( 'NONE', #8303, #7551, #11822, .T. ) ;
#14662 = CARTESIAN_POINT ( 'NONE',  ( 3.082852245407272207, 0.9930332973736890612, 0.3962311736271780793 ) ) ;
#14663 = ORIENTED_EDGE ( 'NONE', *, *, #5029, .F. ) ;
#14664 = CARTESIAN_POINT ( 'NONE',  ( 3.875000000000000000, 0.8660254037844385966, -0.5000000000000002220 ) ) ;
#14665 = DIRECTION ( 'NONE',  ( 0.000000000000000000, 1.000000000000000000, 0.000000000000000000 ) ) ;
#14666 = EDGE_CURVE ( 'NONE', #9754, #8780, #11809, .T. ) ;
#14667 = CARTESIAN_POINT ( 'NONE',  ( 1.532626322880889402, 0.000000000000000000, -0.5400755080658653506 ) ) ;
#14668 = B_SPLINE_CURVE_WITH_KNOTS ( 'NONE', 3,
 ( #5899, #893, #14911, #4438 ),
 .UNSPECIFIED., .F., .F.,
 ( 4, 4 ),
 ( 2.046485264934011349E-07, 0.001800564375689165265 ),
 .UNSPECIFIED. ) ;
#14669 = SURFACE_STYLE_FILL_AREA ( #9161 ) ;
#14670 = CARTESIAN_POINT ( 'NONE',  ( 0.7500000000000001110, 1.000000000000000000, -0.6614378277661475680 ) ) ;
#14671 = DIRECTION ( 'NONE',  ( 0.000000000000000000, 0.000000000000000000, 1.000000000000000000 ) ) ;
#14672 = CONICAL_SURFACE ( 'NONE', #5159, 0.2944999999999856066, 0.7853981633974514986 ) ;
#14673 = CARTESIAN_POINT ( 'NONE',  ( 3.910795929945357408, 1.844675076806764569, 0.7500224038636267299 ) ) ;
#14675 = ORIENTED_EDGE ( 'NONE', *, *, #8764, .T. ) ;
#14674 = CYLINDRICAL_SURFACE ( 'NONE', #1777, 0.2499999999999999167 ) ;
#14676 = EDGE_LOOP ( 'NONE', ( #1337, #3283, #8608, #9100 ) ) ;
#14678 = ORIENTED_EDGE ( 'NONE', *, *, #14455, .T. ) ;
#14677 = CARTESIAN_POINT ( 'NONE',  ( 6.176491571325181340, 1.679378605318035733, -1.679378605318065487 ) ) ;
#14679 =( BOUNDED_SURFACE ( )  B_SPLINE_SURFACE ( 3, 2, ( 
 ( #12012, #10796, #12935 ),
 ( #11507, #4917, #5698 ),
 ( #13000, #286, #9652 ),
 ( #10355, #4547, #14301 ),
 ( #1522, #3837, #7213 ),
 ( #13778, #14074, #1450 ),
 ( #11867, #6057, #13074 ),
 ( #7142, #7359, #15019 ),
 ( #5981, #10721, #2462 ),
 ( #10285, #9584, #7289 ) ),
 .UNSPECIFIED., .F., .F., .F. ) 
 B_SPLINE_SURFACE_WITH_KNOTS ( ( 4, 2, 2, 2, 4 ),
 ( 3, 3 ),
 ( 1.605702911834775426, 1.793325806424166391, 1.980948701013557578, 2.168571595602948765, 2.356194490192339952 ),
 ( 0.000000000000000000, 1.000000000000000000 ),
 .UNSPECIFIED. ) 
 GEOMETRIC_REPRESENTATION_ITEM ( )  RATIONAL_B_SPLINE_SURFACE ( (
 ( 1.000000000000000000, 0.7072810196742752575, 1.000000000000000000),
 ( 1.000000000000000000, 0.7075930366720845077, 1.000000000000000000),
 ( 1.000000000000000000, 0.7079038033994521362, 1.000000000000000000),
 ( 1.000000000000000000, 0.7085120144470745673, 1.000000000000000000),
 ( 1.000000000000000000, 0.7088094415865170417, 1.000000000000000000),
 ( 1.000000000000000000, 0.7093805931376407914, 1.000000000000000000),
 ( 1.000000000000000000, 0.7096543062745851449, 1.000000000000000000),
 ( 1.000000000000000000, 0.7101685202382782558, 1.000000000000000000),
 ( 1.000000000000000000, 0.7104090318599831644, 1.000000000000000000),
 ( 1.000000000000000000, 0.7106287314217426543, 1.000000000000000000) ) ) 
 REPRESENTATION_ITEM ( '' )  SURFACE ( )  );
#14680 = ORIENTED_EDGE ( 'NONE', *, *, #12329, .F. ) ;
#14681 = EDGE_CURVE ( 'NONE', #14331, #14837, #4493, .T. ) ;
#14682 = DIRECTION ( 'NONE',  ( 0.000000000000000000, -1.000000000000000000, 0.000000000000000000 ) ) ;
#14683 = DIRECTION ( 'NONE',  ( 0.000000000000000000, 1.000000000000000000, 0.000000000000000000 ) ) ;
#14684 = EDGE_LOOP ( 'NONE', ( #2587, #13450, #3236, #3882 ) ) ;
#14685 = DIRECTION ( 'NONE',  ( -0.000000000000000000, 1.000000000000000000, -0.000000000000000000 ) ) ;
#14686 = DIRECTION ( 'NONE',  ( 0.000000000000000000, 0.000000000000000000, 1.000000000000000000 ) ) ;
#14687 = EDGE_CURVE ( 'NONE', #13228, #7657, #4857, .T. ) ;
#14688 = CONICAL_SURFACE ( 'NONE', #11999, 0.2945000000000006501, 0.7853981633974503884 ) ;
#14689 = EDGE_CURVE ( 'NONE', #15151, #12880, #15016, .T. ) ;
#14690 = DIRECTION ( 'NONE',  ( -0.4961857140186726189, -0.000000000000000000, -0.8682164115033648155 ) ) ;
#14691 = DIRECTION ( 'NONE',  ( 0.000000000000000000, 0.000000000000000000, 1.000000000000000000 ) ) ;
#14692 = ORIENTED_EDGE ( 'NONE', *, *, #10286, .T. ) ;
#14693 = FACE_OUTER_BOUND ( 'NONE', #9558, .T. ) ;
#14694 = CARTESIAN_POINT ( 'NONE',  ( 3.388167464794443084, 0.9934776249054605435, -0.1151865398313142164 ) ) ;
#14695 = DIRECTION ( 'NONE',  ( -0.7070715176384851919, -0.7070715176384784195, -0.009986885842354102302 ) ) ;
#14696 = EDGE_LOOP ( 'NONE', ( #5977, #15090, #14252, #6330 ) ) ;
#14697 = AXIS2_PLACEMENT_3D ( 'NONE', #12341, #4175, #14792 ) ;
#14698 = DIRECTION ( 'NONE',  ( 0.000000000000000000, 0.000000000000000000, -1.000000000000000000 ) ) ;
#14699 = DIRECTION ( 'NONE',  ( 1.000000000000000000, 0.000000000000000000, 0.000000000000000000 ) ) ;
#14700 = EDGE_LOOP ( 'NONE', ( #13405, #12078, #14702, #4664 ) ) ;
#14701 = CARTESIAN_POINT ( 'NONE',  ( 0.9741570934736516474, -0.4829555140690277582, -0.3620636361668077008 ) ) ;
#14702 = ORIENTED_EDGE ( 'NONE', *, *, #11618, .F. ) ;
#14703 =( CONVERSION_BASED_UNIT ( 'INCH', #8820 ) LENGTH_UNIT ( ) NAMED_UNIT ( #3938 ) );
#14704 = CARTESIAN_POINT ( 'NONE',  ( 3.562574517356508430, 1.987638485117721343, -0.6822768319053587049 ) ) ;
#14705 = EDGE_CURVE ( 'NONE', #11506, #13193, #9526, .T. ) ;
#14706 = CARTESIAN_POINT ( 'NONE',  ( 1.644431316732426263, -0.3408522091762651307, 0.4170406485182424627 ) ) ;
#14707 = CARTESIAN_POINT ( 'NONE',  ( 0.8282270537073739280, -0.4835892651647821783, -0.3529439700516306955 ) ) ;
#14708 = PLANE ( 'NONE',  #3878 ) ;
#14709 = ORIENTED_EDGE ( 'NONE', *, *, #1210, .F. ) ;
#14710 = CARTESIAN_POINT ( 'NONE',  ( 2.650000000000001688, 0.000000000000000000, 0.000000000000000000 ) ) ;
#14711 = CARTESIAN_POINT ( 'NONE',  ( 3.920936730114974456, 1.767235543727864400, 0.7960367706888703543 ) ) ;
#14712 = CARTESIAN_POINT ( 'NONE',  ( 0.7038889044926298633, -0.3873518276109626512, -0.4900580663207255161 ) ) ;
#14713 = ORIENTED_EDGE ( 'NONE', *, *, #10199, .T. ) ;
#14714 = ORIENTED_EDGE ( 'NONE', *, *, #12531, .T. ) ;
#14715 = VECTOR ( 'NONE', #10508, 39.37007874015748143 ) ;
#14716 = DIRECTION ( 'NONE',  ( -0.8702745610686326572, 0.000000000000000000, 0.4925669379452895513 ) ) ;
#14717 = ORIENTED_EDGE ( 'NONE', *, *, #6862, .T. ) ;
#14718 = LINE ( 'NONE', #929, #2802 ) ;
#14719 = CARTESIAN_POINT ( 'NONE',  ( 0.6570985677785624590, -0.3875776804055264257, -0.5130299739594079700 ) ) ;
#14720 = DIRECTION ( 'NONE',  ( 8.659560562355000651E-17, -0.7071067811865421326, 0.7071067811865530128 ) ) ;
#14721 = DIRECTION ( 'NONE',  ( 0.000000000000000000, 0.000000000000000000, 1.000000000000000000 ) ) ;
#14722 = EDGE_CURVE ( 'NONE', #2178, #13224, #8643, .T. ) ;
#14723 = AXIS2_PLACEMENT_3D ( 'NONE', #10054, #2073, #5388 ) ;
#14724 = VERTEX_POINT ( 'NONE', #5855 ) ;
#14725 = ORIENTED_EDGE ( 'NONE', *, *, #1631, .T. ) ;
#14726 = ORIENTED_EDGE ( 'NONE', *, *, #14453, .T. ) ;
#14727 = PRODUCT_DEFINITION_CONTEXT ( 'detailed design', #11536, 'design' ) ;
#14728 = VERTEX_POINT ( 'NONE', #5768 ) ;
#14729 = CARTESIAN_POINT ( 'NONE',  ( 0.2578780456880921390, 1.589927591219149949, -0.3152476286636705649 ) ) ;
#14730 = DIRECTION ( 'NONE',  ( -0.6312257069790480069, 0.000000000000000000, -0.7755991921403740941 ) ) ;
#14731 = CARTESIAN_POINT ( 'NONE',  ( 0.7851380656309442374, -0.4451990772328827672, -0.3237718568205412151 ) ) ;
#14732 = CARTESIAN_POINT ( 'NONE',  ( 0.000000000000000000, 1.603403463250997918, -0.3809527529760087239 ) ) ;
#14733 = EDGE_LOOP ( 'NONE', ( #14318, #9094, #3983, #8232 ) ) ;
#14734 = CARTESIAN_POINT ( 'NONE',  ( 0.2372115730956756152, 0.1749999999999999889, -0.8852856429364902580 ) ) ;
#14735 = DIRECTION ( 'NONE',  ( -1.000000000000000000, -0.000000000000000000, -0.000000000000000000 ) ) ;
#14736 = ADVANCED_FACE ( 'NONE', ( #11579 ), #11657, .F. ) ;
#14737 = EDGE_CURVE ( 'NONE', #14862, #12259, #6450, .T. ) ;
#14738 = LINE ( 'NONE', #6565, #6332 ) ;
#14739 = EDGE_CURVE ( 'NONE', #6953, #6615, #2542, .T. ) ;
#14740 = AXIS2_PLACEMENT_3D ( 'NONE', #5424, #1803, #6493 ) ;
#14741 = AXIS2_PLACEMENT_3D ( 'NONE', #4837, #10644, #7062 ) ;
#14742 = DIRECTION ( 'NONE',  ( 0.3420201433256627732, 0.000000000000000000, -0.9396926207859105373 ) ) ;
#14743 = CARTESIAN_POINT ( 'NONE',  ( 0.8770054111157354892, -0.4307805394128523813, -0.4639681125059474387 ) ) ;
#14744 = ADVANCED_FACE ( 'NONE', ( #4701 ), #7665, .F. ) ;
#14745 = CARTESIAN_POINT ( 'NONE',  ( 3.896946115134541255, 1.794690806442625020, 0.7506982253096490254 ) ) ;
#14747 = ORIENTED_EDGE ( 'NONE', *, *, #8768, .T. ) ;
#14746 = FACE_BOUND ( 'NONE', #9114, .T. ) ;
#14748 = EDGE_LOOP ( 'NONE', ( #11039, #1302, #5117, #14393, #2733, #8715 ) ) ;
#14750 = EDGE_LOOP ( 'NONE', ( #6630, #5731 ) ) ;
#14749 = CARTESIAN_POINT ( 'NONE',  ( 2.372634528609593119, 0.1852128444980909450, -0.4664882128727458888 ) ) ;
#14751 = EDGE_LOOP ( 'NONE', ( #10302, #1458, #2732, #4032 ) ) ;
#14752 = FACE_BOUND ( 'NONE', #7739, .T. ) ;
#14753 = LINE ( 'NONE', #3282, #7461 ) ;
#14754 = ORIENTED_EDGE ( 'NONE', *, *, #3172, .T. ) ;
#14755 = CARTESIAN_POINT ( 'NONE',  ( 0.000000000000000000, 1.866025403784438819, 0.000000000000000000 ) ) ;
#14756 = LINE ( 'NONE', #11163, #5099 ) ;
#14757 = DIRECTION ( 'NONE',  ( 1.000000000000000000, 0.000000000000000000, 0.000000000000000000 ) ) ;
#14758 = AXIS2_PLACEMENT_3D ( 'NONE', #9040, #672, #3370 ) ;
#14759 = CARTESIAN_POINT ( 'NONE',  ( 0.9652173913043480269, -0.4429999999999998939, -0.3379636412230419551 ) ) ;
#14760 = ORIENTED_EDGE ( 'NONE', *, *, #7760, .F. ) ;
#14761 = CARTESIAN_POINT ( 'NONE',  ( -0.7500000000000001110, 1.000000000000000222, -0.6614378277661475680 ) ) ;
#14762 = CARTESIAN_POINT ( 'NONE',  ( 3.582695665244850058, 0.9139351410924635433, -0.4059821268960285834 ) ) ;
#14763 = CARTESIAN_POINT ( 'NONE',  ( 4.531732933946797992, 1.713275703896695701, -0.4642236893194010006 ) ) ;
#14764 = EDGE_CURVE ( 'NONE', #13458, #12462, #4545, .T. ) ;
#14765 = ORIENTED_EDGE ( 'NONE', *, *, #9399, .T. ) ;
#14766 = DIRECTION ( 'NONE',  ( 0.000000000000000000, -1.000000000000000000, 0.000000000000000000 ) ) ;
#14767 = CARTESIAN_POINT ( 'NONE',  ( 2.087921535706059650, 0.2870784642939429587, 0.4105035982572216025 ) ) ;
#14768 = ORIENTED_EDGE ( 'NONE', *, *, #5600, .T. ) ;
#14769 = EDGE_CURVE ( 'NONE', #1386, #39, #10352, .T. ) ;
#14770 = AXIS2_PLACEMENT_3D ( 'NONE', #14158, #1006, #13151 ) ;
#14771 = DIRECTION ( 'NONE',  ( 0.01412288512831583534, 0.000000000000000000, -0.9999002670844989726 ) ) ;
#14772 = ORIENTED_EDGE ( 'NONE', *, *, #1557, .T. ) ;
#14773 = CIRCLE ( 'NONE', #10630, 0.2624999999999994560 ) ;
#14774 = DIRECTION ( 'NONE',  ( 0.000000000000000000, 0.000000000000000000, -1.000000000000000000 ) ) ;
#14775 = DIRECTION ( 'NONE',  ( -1.000000000000000000, -0.000000000000000000, -0.000000000000000000 ) ) ;
#14776 = DIRECTION ( 'NONE',  ( -1.000000000000000000, -0.000000000000000000, -0.000000000000000000 ) ) ;
#14777 = VERTEX_POINT ( 'NONE', #2399 ) ;
#14778 = VECTOR ( 'NONE', #2363, 39.37007874015748143 ) ;
#14779 = CARTESIAN_POINT ( 'NONE',  ( 6.176491571325181340, 1.679378605318035733, -1.679378605318065487 ) ) ;
#14780 = CARTESIAN_POINT ( 'NONE',  ( 3.629736278057476007, 1.863380661955394091, 0.7703184054743784648 ) ) ;
#14781 = VECTOR ( 'NONE', #2280, 39.37007874015748143 ) ;
#14782 = AXIS2_PLACEMENT_3D ( 'NONE', #2993, #5446, #3221 ) ;
#14783 = SURFACE_SIDE_STYLE ('',( #6010 ) ) ;
#14784 = DIRECTION ( 'NONE',  ( -1.000000000000000000, -2.130223169792495565E-16, 0.000000000000000000 ) ) ;
#14785 = VERTEX_POINT ( 'NONE', #2242 ) ;
#14786 = ORIENTED_EDGE ( 'NONE', *, *, #3634, .T. ) ;
#14787 = EDGE_CURVE ( 'NONE', #969, #539, #10112, .T. ) ;
#14788 = EDGE_CURVE ( 'NONE', #5479, #6020, #9624, .T. ) ;
#14789 = CARTESIAN_POINT ( 'NONE',  ( 3.426491571325181340, 0.000000000000000000, 0.000000000000000000 ) ) ;
#14790 = EDGE_LOOP ( 'NONE', ( #2343, #8284, #10586, #4678 ) ) ;
#14791 = LINE ( 'NONE', #1855, #11598 ) ;
#14792 = DIRECTION ( 'NONE',  ( 1.092739197465705485E-15, 0.000000000000000000, -1.000000000000000000 ) ) ;
#14793 = CIRCLE ( 'NONE', #3070, 0.3750000000000004996 ) ;
#14794 = DIRECTION ( 'NONE',  ( 0.000000000000000000, 0.000000000000000000, -1.000000000000000000 ) ) ;
#14795 = AXIS2_PLACEMENT_3D ( 'NONE', #5050, #14361, #8356 ) ;
#14796 = VECTOR ( 'NONE', #10759, 39.37007874015748143 ) ;
#14797 = CARTESIAN_POINT ( 'NONE',  ( 2.061999999999999833, 2.257636374228145754E-16, 1.812000000000000277 ) ) ;
#14798 = ORIENTED_EDGE ( 'NONE', *, *, #7281, .T. ) ;
#14799 = CARTESIAN_POINT ( 'NONE',  ( -5.764454660286586870E-18, -0.2214999999999999469, 0.000000000000000000 ) ) ;
#14800 = AXIS2_PLACEMENT_3D ( 'NONE', #8794, #13285, #12077 ) ;
#14801 = CARTESIAN_POINT ( 'NONE',  ( 4.214877066107062475, 1.735343601526363022, -0.6696222561766873582 ) ) ;
#14802 = VERTEX_POINT ( 'NONE', #4625 ) ;
#14803 = VECTOR ( 'NONE', #1320, 39.37007874015748143 ) ;
#14804 = VERTEX_POINT ( 'NONE', #9298 ) ;
#14805 = AXIS2_PLACEMENT_3D ( 'NONE', #7756, #11343, #13631 ) ;
#14806 = ORIENTED_EDGE ( 'NONE', *, *, #12485, .T. ) ;
#14807 = DIRECTION ( 'NONE',  ( 0.000000000000000000, -1.000000000000000000, 0.000000000000000000 ) ) ;
#14808 = LINE ( 'NONE', #14888, #8967 ) ;
#14809 = CARTESIAN_POINT ( 'NONE',  ( 0.7926600297304221554, -0.4443591734166930096, -0.3139846204486113623 ) ) ;
#14810 = ITEM_DEFINED_TRANSFORMATION ( 'NONE', 'NONE', #13510,  #8424 ) ;
#14811 = CARTESIAN_POINT ( 'NONE',  ( -0.1266950372298287220, 1.593635284016129194, 0.3809527529760087239 ) ) ;
#14812 = ORIENTED_EDGE ( 'NONE', *, *, #233, .F. ) ;
#14813 = CARTESIAN_POINT ( 'NONE',  ( 2.633946444925666874, 0.3625193201794746356, 0.4033906250602100618 ) ) ;
#14814 = AXIS2_PLACEMENT_3D ( 'NONE', #10468, #7039, #2441 ) ;
#14815 = CARTESIAN_POINT ( 'NONE',  ( 0.6746175797782247852, -0.05587126532790559486, -0.4907030699473264868 ) ) ;
#14816 = CIRCLE ( 'NONE', #11661, 0.07500000000000002498 ) ;
#14817 = DIRECTION ( 'NONE',  ( 1.000000000000000000, 0.000000000000000000, 0.000000000000000000 ) ) ;
#14818 = CARTESIAN_POINT ( 'NONE',  ( 4.292613398383279488, 1.780257219922917411, 0.6242760036277545943 ) ) ;
#14819 = EDGE_CURVE ( 'NONE', #3024, #10523, #12053, .T. ) ;
#14821 = EDGE_LOOP ( 'NONE', ( #15010, #14422, #11359, #10772 ) ) ;
#14820 = CARTESIAN_POINT ( 'NONE',  ( 2.980731298636167370, 3.137999999999999901, -0.3249191361593797844 ) ) ;
#14822 = AXIS2_PLACEMENT_3D ( 'NONE', #11521, #4563, #1326 ) ;
#14823 = EDGE_LOOP ( 'NONE', ( #5801, #3482, #9255, #10934 ) ) ;
#14825 = EDGE_LOOP ( 'NONE', ( #1366, #10835, #10045, #14128 ) ) ;
#14824 = CARTESIAN_POINT ( 'NONE',  ( 0.3724999999999999423, -0.6589999999999996971, 0.3724999999999999423 ) ) ;
#14826 = EDGE_LOOP ( 'NONE', ( #9176, #6850, #3273, #4479, #1846, #12590, #1496, #14012, #1116, #8750, #3960, #6680, #6883 ) ) ;
#14827 = DIRECTION ( 'NONE',  ( 0.000000000000000000, 1.000000000000000000, 0.000000000000000000 ) ) ;
#14828 = DIRECTION ( 'NONE',  ( -1.000000000000000000, -0.000000000000000000, -0.000000000000000000 ) ) ;
#14829 = ORIENTED_EDGE ( 'NONE', *, *, #10338, .T. ) ;
#14830 = AXIS2_PLACEMENT_3D ( 'NONE', #12356, #9153, #3113 ) ;
#14831 = DIRECTION ( 'NONE',  ( -1.000000000000000000, -0.000000000000000000, -0.000000000000000000 ) ) ;
#14832 = CARTESIAN_POINT ( 'NONE',  ( 2.774999999999999911, 1.679378605318059048, 1.679378605318041506 ) ) ;
#14833 = EDGE_CURVE ( 'NONE', #13435, #5151, #3511, .T. ) ;
#14834 = LINE ( 'NONE', #8117, #14013 ) ;
#14835 = DIRECTION ( 'NONE',  ( 0.000000000000000000, 0.000000000000000000, -1.000000000000000000 ) ) ;
#14836 = CARTESIAN_POINT ( 'NONE',  ( 1.014392645310246754, -0.4429482298831206033, -0.3623584098607407489 ) ) ;
#14837 = VERTEX_POINT ( 'NONE', #1468 ) ;
#14838 = DIRECTION ( 'NONE',  ( 0.000000000000000000, 0.000000000000000000, 1.000000000000000000 ) ) ;
#14839 = CARTESIAN_POINT ( 'NONE',  ( 3.808373759217316579, 0.8679908749363488552, -0.4966365464873185309 ) ) ;
#14840 = EDGE_CURVE ( 'NONE', #7567, #6113, #11210, .T. ) ;
#14841 = VECTOR ( 'NONE', #12142, 39.37007874015748143 ) ;
#14842 = FACE_OUTER_BOUND ( 'NONE', #676, .T. ) ;
#14843 = EDGE_CURVE ( 'NONE', #11355, #14657, #10490, .T. ) ;
#14844 = CARTESIAN_POINT ( 'NONE',  ( 4.239713504559157187, 0.9396297378138827039, -0.3424101421577204207 ) ) ;
#14845 = CARTESIAN_POINT ( 'NONE',  ( 0.6500000000000001332, 1.504103507210760471, 0.000000000000000000 ) ) ;
#14846 = VERTEX_POINT ( 'NONE', #2927 ) ;
#14847 = DIRECTION ( 'NONE',  ( 0.000000000000000000, 0.000000000000000000, -1.000000000000000000 ) ) ;
#14848 = DIRECTION ( 'NONE',  ( 0.000000000000000000, 0.000000000000000000, -1.000000000000000000 ) ) ;
#14849 = VECTOR ( 'NONE', #15098, 39.37007874015748143 ) ;
#14850 = EDGE_CURVE ( 'NONE', #4070, #11468, #14254, .T. ) ;
#14851 = AXIS2_PLACEMENT_3D ( 'NONE', #10643, #14072, #1368 ) ;
#14852 = EDGE_CURVE ( 'NONE', #5216, #1024, #1513, .T. ) ;
#14853 = CARTESIAN_POINT ( 'NONE',  ( 0.7429783265673733927, -0.4429999999999999494, -0.4366554833170141481 ) ) ;
#14854 = FACE_OUTER_BOUND ( 'NONE', #1174, .T. ) ;
#14855 = AXIS2_PLACEMENT_3D ( 'NONE', #2988, #10261, #12609 ) ;
#14856 = CARTESIAN_POINT ( 'NONE',  ( 0.6500000000000001332, 0.000000000000000000, 0.000000000000000000 ) ) ;
#14857 = VERTEX_POINT ( 'NONE', #13094 ) ;
#14858 = VECTOR ( 'NONE', #250, 39.37007874015748143 ) ;
#14859 = CARTESIAN_POINT ( 'NONE',  ( 2.774999999999999911, -2.360000000000016751, -1.574999999999999956 ) ) ;
#14860 = CARTESIAN_POINT ( 'NONE',  ( 0.8293581428695305791, -0.4837316503856468053, -0.3495487851854117145 ) ) ;
#14861 = CARTESIAN_POINT ( 'NONE',  ( 6.176491571325181340, -1.679378605318048390, 1.679378605318054163 ) ) ;
#14862 = VERTEX_POINT ( 'NONE', #13232 ) ;
#14863 = EDGE_LOOP ( 'NONE', ( #5707, #13089, #10095, #7220 ) ) ;
#14864 = LINE ( 'NONE', #4397, #12973 ) ;
#14865 = DIRECTION ( 'NONE',  ( 0.000000000000000000, 0.000000000000000000, 1.000000000000000000 ) ) ;
#14866 = EDGE_LOOP ( 'NONE', ( #11366, #10843, #8590, #12863 ) ) ;
#14867 = DIRECTION ( 'NONE',  ( -1.000000000000000000, -0.000000000000000000, -0.000000000000000000 ) ) ;
#14868 = VECTOR ( 'NONE', #1456, 39.37007874015748143 ) ;
#14869 = VECTOR ( 'NONE', #13281, 39.37007874015748143 ) ;
#14870 = ADVANCED_FACE ( 'NONE', ( #8596, #2771 ), #6299, .T. ) ;
#14871 = CARTESIAN_POINT ( 'NONE',  ( 0.6734800455634237792, -0.4130371149665958419, -0.4827503109326044539 ) ) ;
#14872 = AXIS2_PLACEMENT_3D ( 'NONE', #1232, #8377, #5921 ) ;
#14873 = CARTESIAN_POINT ( 'NONE',  ( 2.807000000000000384, 1.679378605318059048, 1.416878605318041551 ) ) ;
#14874 = AXIS2_PLACEMENT_3D ( 'NONE', #5814, #10251, #2366 ) ;
#14875 = AXIS2_PLACEMENT_3D ( 'NONE', #13428, #11296, #2963 ) ;
#14876 = CARTESIAN_POINT ( 'NONE',  ( 2.774999999999999911, 3.360000000000000320, -0.9800000000000012035 ) ) ;
#14877 = EDGE_CURVE ( 'NONE', #1691, #13670, #3267, .T. ) ;
#14878 = ORIENTED_EDGE ( 'NONE', *, *, #343, .F. ) ;
#14879 = FACE_OUTER_BOUND ( 'NONE', #8656, .T. ) ;
#14880 = COLOUR_RGB ( '',0.7921568627450980005, 0.8196078431372548767, 0.9333333333333333481 ) ;
#14881 = CARTESIAN_POINT ( 'NONE',  ( 3.827026189994130245, 1.815548848758673506, -0.7493866505369201070 ) ) ;
#14882 = ORIENTED_EDGE ( 'NONE', *, *, #147, .F. ) ;
#14883 = ORIENTED_EDGE ( 'NONE', *, *, #3764, .F. ) ;
#14884 = PRODUCT_DEFINITION_CONTEXT ( 'detailed design', #4500, 'design' ) ;
#14885 = CARTESIAN_POINT ( 'NONE',  ( -0.3389861398595948039, 1.603403919227001762, -0.1747642886535499263 ) ) ;
#14886 = VERTEX_POINT ( 'NONE', #12468 ) ;
#14887 = DIRECTION ( 'NONE',  ( 0.000000000000000000, 0.000000000000000000, 1.000000000000000000 ) ) ;
#14888 = CARTESIAN_POINT ( 'NONE',  ( -0.2099999999999999922, 0.7512260236060024354, 0.3809527529760087239 ) ) ;
#14889 = CARTESIAN_POINT ( 'NONE',  ( 0.7811313390194075668, -0.4446478369844531486, -0.3386457300789465497 ) ) ;
#14890 = DIRECTION ( 'NONE',  ( 0.000000000000000000, 0.000000000000000000, -1.000000000000000000 ) ) ;
#14891 = ORIENTED_EDGE ( 'NONE', *, *, #14661, .F. ) ;
#14892 = CARTESIAN_POINT ( 'NONE',  ( 3.126543437434640804, 2.500005182251167746, -0.01362379177072846510 ) ) ;
#14893 = CARTESIAN_POINT ( 'NONE',  ( -0.3725000000000000533, -0.6290000000000005587, 0.3724999999999999423 ) ) ;
#14894 = FACE_OUTER_BOUND ( 'NONE', #10989, .T. ) ;
#14895 = TOROIDAL_SURFACE ( 'NONE', #5134, 0.3439999999999999170, 0.1068000000000000754 ) ;
#14896 = ADVANCED_FACE ( 'NONE', ( #908 ), #827, .F. ) ;
#14897 = CARTESIAN_POINT ( 'NONE',  ( 3.874999999999999556, 3.137999999999999901, 1.320000000000000062 ) ) ;
#14898 = CARTESIAN_POINT ( 'NONE',  ( 4.231255996368110672, 1.713208384118555250, 0.7116634002984181251 ) ) ;
#14900 = VERTEX_POINT ( 'NONE', #12396 ) ;
#14899 = CARTESIAN_POINT ( 'NONE',  ( 0.6180000000000012150, 0.000000000000000000, 3.000000000000000444 ) ) ;
#14901 = ORIENTED_EDGE ( 'NONE', *, *, #4389, .T. ) ;
#14903 = VERTEX_POINT ( 'NONE', #2997 ) ;
#14902 = DIRECTION ( 'NONE',  ( 0.7070715176384863021, 0.7070715176384774203, 0.009986885842351498482 ) ) ;
#14904 = ORIENTED_EDGE ( 'NONE', *, *, #5210, .T. ) ;
#14905 = CARTESIAN_POINT ( 'NONE',  ( 2.124999999999999556, -0.9799999999999436939, 3.360000000000016751 ) ) ;
#14906 = DIRECTION ( 'NONE',  ( 0.03462124711964004870, 3.234772430654374379E-16, -0.9994005049267692398 ) ) ;
#14907 = DIRECTION ( 'NONE',  ( 0.01412288512831213171, -3.675428035873182550E-19, 0.9999002670844991947 ) ) ;
#14908 = EDGE_LOOP ( 'NONE', ( #4851, #13777, #2873, #11862 ) ) ;
#14909 = CARTESIAN_POINT ( 'NONE',  ( 0.7856509485162611606, -0.4429999999999998939, -0.3627813902276396663 ) ) ;
#14910 = LINE ( 'NONE', #10321, #10483 ) ;
#14911 = CARTESIAN_POINT ( 'NONE',  ( 3.897996994672882742, 1.878547046383948205, 0.4999999999999717448 ) ) ;
#14912 = DIRECTION ( 'NONE',  ( 0.7071067811865452413, 0.000000000000000000, -0.7071067811865497932 ) ) ;
#14913 = CARTESIAN_POINT ( 'NONE',  ( 2.715114969687650870, 0.8546659208687416021, -0.4012693820656907939 ) ) ;
#14914 = PRODUCT_DEFINITION ( 'UNKNOWN', '', #12555, #8163 ) ;
#14915 = CARTESIAN_POINT ( 'NONE',  ( 2.774999999999999911, -1.679378605318041950, 1.384878605318059064 ) ) ;
#14916 = VERTEX_POINT ( 'NONE', #12541 ) ;
#14917 = DIRECTION ( 'NONE',  ( 0.000000000000000000, 0.000000000000000000, -1.000000000000000000 ) ) ;
#14918 = DIRECTION ( 'NONE',  ( 0.000000000000000000, 1.000000000000000000, 0.000000000000000000 ) ) ;
#14919 = DIRECTION ( 'NONE',  ( -0.000000000000000000, -1.000000000000000000, -0.000000000000000000 ) ) ;
#14920 = CARTESIAN_POINT ( 'NONE',  ( 0.000000000000000000, 0.000000000000000000, -0.4999999999999997224 ) ) ;
#14922 = ORIENTED_EDGE ( 'NONE', *, *, #5888, .F. ) ;
#14921 = CARTESIAN_POINT ( 'NONE',  ( 2.774999999999999911, 1.574999999999994849, -1.575000000000022160 ) ) ;
#14923 = ORIENTED_EDGE ( 'NONE', *, *, #7569, .T. ) ;
#14924 = DIRECTION ( 'NONE',  ( -1.874307916738606601E-16, 1.000000000000000000, 0.000000000000000000 ) ) ;
#14925 = VERTEX_POINT ( 'NONE', #6519 ) ;
#14926 = MECHANICAL_DESIGN_GEOMETRIC_PRESENTATION_REPRESENTATION (  '', ( #4671 ), #11017 ) ;
#14927 = DIRECTION ( 'NONE',  ( 0.000000000000000000, 0.000000000000000000, -1.000000000000000000 ) ) ;
#14928 = CARTESIAN_POINT ( 'NONE',  ( 3.426491571325181340, -2.360000000000000320, 0.9799999999999999822 ) ) ;
#14929 = ADVANCED_FACE ( 'NONE', ( #11175 ), #5379, .F. ) ;
#14930 = EDGE_CURVE ( 'NONE', #3525, #2976, #11102, .T. ) ;
#14931 = DIRECTION ( 'NONE',  ( 0.000000000000000000, -1.000000000000000000, 1.423315761404775650E-14 ) ) ;
#14932 = CARTESIAN_POINT ( 'NONE',  ( 2.650000000000001688, 1.224646799147353207E-16, -1.000000000000000000 ) ) ;
#14933 = EDGE_CURVE ( 'NONE', #4870, #9754, #3997, .T. ) ;
#14934 = DIRECTION ( 'NONE',  ( 3.491481338843132961E-15, 0.000000000000000000, -1.000000000000000000 ) ) ;
#14935 = VERTEX_POINT ( 'NONE', #5607 ) ;
#14936 = CARTESIAN_POINT ( 'NONE',  ( 2.371787155501894784, 0.1852128444980909727, 0.4064941968476759038 ) ) ;
#14937 = CIRCLE ( 'NONE', #1975, 0.7849999999999996980 ) ;
#14938 = DIRECTION ( 'NONE',  ( 0.000000000000000000, 0.000000000000000000, -1.000000000000000000 ) ) ;
#14939 = EDGE_CURVE ( 'NONE', #6203, #2093, #10677, .T. ) ;
#14940 = CARTESIAN_POINT ( 'NONE',  ( 0.7095752389709895080, -0.4273810847934926826, -0.4705416541824789523 ) ) ;
#14941 = VERTEX_POINT ( 'NONE', #1756 ) ;
#14942 = DIRECTION ( 'NONE',  ( -1.874307916738608820E-16, 1.000000000000000000, 0.000000000000000000 ) ) ;
#14943 = CARTESIAN_POINT ( 'NONE',  ( 6.208491571325183145, -1.679378605318048390, 1.679378605318054163 ) ) ;
#14944 = DIRECTION ( 'NONE',  ( 1.000000000000000000, 0.000000000000000000, 0.000000000000000000 ) ) ;
#14945 = ORIENTED_EDGE ( 'NONE', *, *, #11494, .F. ) ;
#14946 = DIRECTION ( 'NONE',  ( 0.000000000000000000, 0.000000000000000000, -1.000000000000000000 ) ) ;
#14947 = CARTESIAN_POINT ( 'NONE',  ( 0.6558077255084636681, -0.4243582046485735448, -0.5013227096633714464 ) ) ;
#14948 = CARTESIAN_POINT ( 'NONE',  ( 3.874999999999999556, 3.137999999999999901, 1.320000000000000062 ) ) ;
#14949 = CARTESIAN_POINT ( 'NONE',  ( 3.759712767994416893, 1.920664053109024660, 0.4870725753588067697 ) ) ;
#14950 = ORIENTED_EDGE ( 'NONE', *, *, #3355, .F. ) ;
#14951 = DIRECTION ( 'NONE',  ( -1.000000000000000000, -0.000000000000000000, -0.000000000000000000 ) ) ;
#14952 = ADVANCED_BREP_SHAPE_REPRESENTATION ( '', ( #10666, #8424 ), #3278 ) ;
#14953 = CARTESIAN_POINT ( 'NONE',  ( 3.563625566911128750, 1.891043865854203920, -0.7492590735562228987 ) ) ;
#14954 = ORIENTED_EDGE ( 'NONE', *, *, #3371, .F. ) ;
#14955 = ORIENTED_EDGE ( 'NONE', *, *, #995, .F. ) ;
#14956 = ADVANCED_FACE ( 'NONE', ( #7661 ), #13532, .T. ) ;
#14957 = CARTESIAN_POINT ( 'NONE',  ( -0.2447605936724017717, 1.581084130983674951, -0.3379677220206969146 ) ) ;
#14958 = ORIENTED_EDGE ( 'NONE', *, *, #2538, .T. ) ;
#14959 = CARTESIAN_POINT ( 'NONE',  ( 0.2249147617188371751, 1.559103846021539619, -0.3723417112827391295 ) ) ;
#14960 = CARTESIAN_POINT ( 'NONE',  ( 2.774999999999999911, 0.000000000000000000, -1.124999999999998446 ) ) ;
#14961 = DIRECTION ( 'NONE',  ( 0.9999002670844989726, 0.000000000000000000, 0.01412288512831212997 ) ) ;
#14962 = EDGE_CURVE ( 'NONE', #14153, #11308, #548, .T. ) ;
#14963 = CARTESIAN_POINT ( 'NONE',  ( 0.1702344636782991416, 1.581111061277887808, -0.3809527529760087794 ) ) ;
#14964 = ORIENTED_EDGE ( 'NONE', *, *, #10391, .T. ) ;
#14965 = CARTESIAN_POINT ( 'NONE',  ( 2.124999999999999556, 1.679378605318042395, -1.679378605318058604 ) ) ;
#14966 = CIRCLE ( 'NONE', #1512, 0.2624999999999997335 ) ;
#14967 = CARTESIAN_POINT ( 'NONE',  ( 0.6782634401674636493, -0.01315021828653769632, -0.4690018541713429356 ) ) ;
#14968 = DIRECTION ( 'NONE',  ( 1.000000000000000000, 0.000000000000000000, 0.000000000000000000 ) ) ;
#14969 = DIRECTION ( 'NONE',  ( 0.000000000000000000, 0.000000000000000000, -1.000000000000000000 ) ) ;
#14970 = CARTESIAN_POINT ( 'NONE',  ( 4.623575768221273030, 1.748705500634446297, -0.06916614078429211832 ) ) ;
#14972 = ORIENTED_EDGE ( 'NONE', *, *, #14383, .F. ) ;
#14971 = DIRECTION ( 'NONE',  ( 0.000000000000000000, 0.000000000000000000, -1.000000000000000000 ) ) ;
#14973 = ORIENTED_EDGE ( 'NONE', *, *, #12813, .T. ) ;
#14975 = ORIENTED_EDGE ( 'NONE', *, *, #3381, .F. ) ;
#14974 = DIRECTION ( 'NONE',  ( 0.000000000000000000, 1.000000000000000000, 0.000000000000000000 ) ) ;
#14976 = VERTEX_POINT ( 'NONE', #3225 ) ;
#14977 = EDGE_CURVE ( 'NONE', #5232, #12211, #7656, .T. ) ;
#14978 = LINE ( 'NONE', #9029, #7053 ) ;
#14979 = EDGE_CURVE ( 'NONE', #167, #5151, #11328, .T. ) ;
#14980 = DIRECTION ( 'NONE',  ( -1.083031686670339959E-16, 0.5429356383595238533, 0.8397743105139239272 ) ) ;
#14981 = DIRECTION ( 'NONE',  ( -1.000000000000000000, -0.000000000000000000, -0.000000000000000000 ) ) ;
#14982 = ORIENTED_EDGE ( 'NONE', *, *, #10119, .F. ) ;
#14983 = CIRCLE ( 'NONE', #8403, 0.9499999999999988454 ) ;
#14984 = CARTESIAN_POINT ( 'NONE',  ( 6.794491571325179891, -1.679378605318047946, -1.304378605318053053 ) ) ;
#14985 = DIRECTION ( 'NONE',  ( 0.000000000000000000, 0.000000000000000000, -1.000000000000000000 ) ) ;
#14986 = FACE_OUTER_BOUND ( 'NONE', #7849, .T. ) ;
#14987 = CARTESIAN_POINT ( 'NONE',  ( 2.774999999999999911, -1.679378605318059048, -1.679378605318041950 ) ) ;
#14988 = ORIENTED_EDGE ( 'NONE', *, *, #8522, .F. ) ;
#14989 = DIRECTION ( 'NONE',  ( -1.000000000000000000, -0.000000000000000000, -0.000000000000000000 ) ) ;
#14990 = AXIS2_PLACEMENT_3D ( 'NONE', #5666, #9104, #11474 ) ;
#14991 = DIRECTION ( 'NONE',  ( 1.000000000000000000, 0.000000000000000000, 0.000000000000000000 ) ) ;
#14992 = CARTESIAN_POINT ( 'NONE',  ( 4.180771277348069859, 1.718521109949383785, -0.7338151851141401227 ) ) ;
#14993 = AXIS2_PLACEMENT_3D ( 'NONE', #13936, #6923, #7159 ) ;
#14994 = DIRECTION ( 'NONE',  ( 0.000000000000000000, 0.000000000000000000, 1.000000000000000000 ) ) ;
#14996 = VERTEX_POINT ( 'NONE', #9965 ) ;
#14995 = CARTESIAN_POINT ( 'NONE',  ( 3.874999999999999556, 3.137999999999999901, -1.509999999999999787 ) ) ;
#14997 = ORIENTED_EDGE ( 'NONE', *, *, #3764, .T. ) ;
#14998 = CYLINDRICAL_SURFACE ( 'NONE', #14014, 0.03999999999999998002 ) ;
#14999 = ORIENTED_EDGE ( 'NONE', *, *, #7036, .F. ) ;
#15000 = EDGE_CURVE ( 'NONE', #13586, #11914, #4740, .T. ) ;
#15001 = DIRECTION ( 'NONE',  ( 0.000000000000000000, -1.000000000000000000, 0.000000000000000000 ) ) ;
#15002 = CARTESIAN_POINT ( 'NONE',  ( 3.112533253352848028, 0.6487563425743168022, -0.3962704070063717832 ) ) ;
#15003 = AXIS2_PLACEMENT_3D ( 'NONE', #7806, #12459, #12124 ) ;
#15004 = AXIS2_PLACEMENT_3D ( 'NONE', #7288, #9583, #13073 ) ;
#15005 = CARTESIAN_POINT ( 'NONE',  ( 2.156999999999999140, -1.679378605318041950, 1.679378605318059048 ) ) ;
#15006 = CYLINDRICAL_SURFACE ( 'NONE', #11452, 0.05999999999999994227 ) ;
#15007 = VERTEX_POINT ( 'NONE', #5291 ) ;
#15008 = CARTESIAN_POINT ( 'NONE',  ( 0.7013557507355877574, -0.4108899945127513220, 0.4833783981792030837 ) ) ;
#15009 = CARTESIAN_POINT ( 'NONE',  ( 0.6773491704061629370, -0.2214999999999999469, 0.5135154343835076629 ) ) ;
#15010 = ORIENTED_EDGE ( 'NONE', *, *, #3641, .F. ) ;
#15011 = CIRCLE ( 'NONE', #4771, 0.4999999999999997224 ) ;
#15012 = DIRECTION ( 'NONE',  ( 0.7071067811865501263, 8.659560562354900811E-17, 0.7071067811865449082 ) ) ;
#15013 = ORIENTED_EDGE ( 'NONE', *, *, #8540, .F. ) ;
#15014 = ADVANCED_FACE ( 'NONE', ( #9116 ), #753, .T. ) ;
#15015 = ADVANCED_FACE ( 'NONE', ( #4303 ), #14623, .T. ) ;
#15016 = LINE ( 'NONE', #2479, #6936 ) ;
#15017 = ORIENTED_EDGE ( 'NONE', *, *, #7536, .T. ) ;
#15018 = ADVANCED_FACE ( 'NONE', ( #13613 ), #4246, .F. ) ;
#15019 = CARTESIAN_POINT ( 'NONE',  ( 2.738128344600763597, 0.4573395005111794420, 0.4018406495282661473 ) ) ;
#15020 = DIRECTION ( 'NONE',  ( 1.000000000000000000, 0.000000000000000000, 0.000000000000000000 ) ) ;
#15021 = CARTESIAN_POINT ( 'NONE',  ( 0.8117875299037612402, -0.4418393224706574363, -0.4412646976173770774 ) ) ;
#15022 = ADVANCED_FACE ( 'NONE', ( #4382 ), #6204, .F. ) ;
#15023 = TOROIDAL_SURFACE ( 'NONE', #3793, 0.7173254825712083171, 0.05999999999999999778 ) ;
#15024 = CARTESIAN_POINT ( 'NONE',  ( 4.170088648937899656, 1.789706488608662216, -0.6902842372149408101 ) ) ;
#15025 = VECTOR ( 'NONE', #5303, 39.37007874015748143 ) ;
#15026 = AXIS2_PLACEMENT_3D ( 'NONE', #7217, #11944, #13999 ) ;
#15027 = DIRECTION ( 'NONE',  ( -1.000000000000000000, -0.000000000000000000, -0.000000000000000000 ) ) ;
#15028 = ORIENTED_EDGE ( 'NONE', *, *, #10795, .T. ) ;
#15029 = EDGE_CURVE ( 'NONE', #8673, #6601, #4685, .T. ) ;
#15030 = ORIENTED_EDGE ( 'NONE', *, *, #3419, .F. ) ;
#15031 = UNCERTAINTY_MEASURE_WITH_UNIT (LENGTH_MEASURE( 1.000000000000000082E-05 ), #11158, 'distance_accuracy_value', 'NONE');
#15032 = CARTESIAN_POINT ( 'NONE',  ( 3.426491571325181340, 0.000000000000000000, 0.000000000000000000 ) ) ;
#15033 = EDGE_LOOP ( 'NONE', ( #5129, #444, #4060, #3582 ) ) ;
#15034 = EDGE_CURVE ( 'NONE', #13231, #14886, #12536, .T. ) ;
#15035 = CARTESIAN_POINT ( 'NONE',  ( 2.156999999999999584, 1.679378605318042395, -1.679378605318058604 ) ) ;
#15036 = VECTOR ( 'NONE', #6429, 39.37007874015748143 ) ;
#15037 = AXIS2_PLACEMENT_3D ( 'NONE', #3756, #12007, #8426 ) ;
#15038 = DIRECTION ( 'NONE',  ( -0.9396926207859107594, 0.000000000000000000, -0.3420201433256624401 ) ) ;
#15039 = CARTESIAN_POINT ( 'NONE',  ( 0.000000000000000000, 1.239999999999999991, 0.000000000000000000 ) ) ;
#15040 = CARTESIAN_POINT ( 'NONE',  ( 1.250000000000000000, -0.05999999999999979655, 0.4223386481965726857 ) ) ;
#15041 = ORIENTED_EDGE ( 'NONE', *, *, #4178, .F. ) ;
#15042 = CARTESIAN_POINT ( 'NONE',  ( 3.193454851037015985, 2.480721379492803358, 0.3109605352214736551 ) ) ;
#15043 = CARTESIAN_POINT ( 'NONE',  ( 0.6610203958102899291, 0.006418471913053761316, -0.4833908188384093974 ) ) ;
#15044 = DIRECTION ( 'NONE',  ( 0.000000000000000000, 0.000000000000000000, -1.000000000000000000 ) ) ;
#15045 = ADVANCED_FACE ( 'NONE', ( #10568 ), #14998, .F. ) ;
#15046 = VECTOR ( 'NONE', #2055, 39.37007874015748854 ) ;
#15047 = AXIS2_PLACEMENT_3D ( 'NONE', #8246, #172, #5783 ) ;
#15048 = CARTESIAN_POINT ( 'NONE',  ( 0.000000000000000000, 1.610000000000000098, 0.000000000000000000 ) ) ;
#15049 = EDGE_CURVE ( 'NONE', #10543, #15127, #2554, .T. ) ;
#15050 = CARTESIAN_POINT ( 'NONE',  ( 4.616151631548642165, 1.808401919742543607, 0.1257952528007890425 ) ) ;
#15052 = ORIENTED_EDGE ( 'NONE', *, *, #13440, .F. ) ;
#15051 = CARTESIAN_POINT ( 'NONE',  ( 3.874999999999999556, 3.567999999999999616, -1.320000000000000062 ) ) ;
#15053 = EDGE_LOOP ( 'NONE', ( #13472, #15134, #6458, #11280 ) ) ;
#15055 = VERTEX_POINT ( 'NONE', #3454 ) ;
#15054 = DIRECTION ( 'NONE',  ( -1.000000000000000000, -1.874307916738609066E-16, 0.000000000000000000 ) ) ;
#15056 = ORIENTED_EDGE ( 'NONE', *, *, #2856, .T. ) ;
#15057 = CARTESIAN_POINT ( 'NONE',  ( 3.394491571325183088, 1.679378605318059048, 1.416878605318041551 ) ) ;
#15058 = VECTOR ( 'NONE', #9860, 39.37007874015748143 ) ;
#15059 = DIRECTION ( 'NONE',  ( 3.779312718515659280E-16, 0.000000000000000000, 1.000000000000000000 ) ) ;
#15060 = ORIENTED_EDGE ( 'NONE', *, *, #6754, .F. ) ;
#15061 = CYLINDRICAL_SURFACE ( 'NONE', #14104, 0.4850000000000000422 ) ;
#15062 = DIRECTION ( 'NONE',  ( 0.000000000000000000, 0.000000000000000000, 1.000000000000000000 ) ) ;
#15063 = LINE ( 'NONE', #3596, #8080 ) ;
#15064 = CARTESIAN_POINT ( 'NONE',  ( 0.000000000000000000, -1.002374524060224757E-18, 0.1520000000000001905 ) ) ;
#15065 = CARTESIAN_POINT ( 'NONE',  ( 3.874999999999999556, 3.137999999999999901, 1.320000000000000062 ) ) ;
#15066 = CARTESIAN_POINT ( 'NONE',  ( -0.2849999999999999756, 5.750000472440944144, -0.4108223460329293864 ) ) ;
#15067 = ADVANCED_FACE ( 'NONE', ( #986 ), #3529, .T. ) ;
#15068 = DIRECTION ( 'NONE',  ( -1.000000000000000000, -0.000000000000000000, -0.000000000000000000 ) ) ;
#15069 = EDGE_CURVE ( 'NONE', #12293, #10863, #6460, .T. ) ;
#15070 = TOROIDAL_SURFACE ( 'NONE', #2372, 0.1150000000000000050, 0.04000000000000000083 ) ;
#15071 = LINE ( 'NONE', #4596, #1905 ) ;
#15072 = CARTESIAN_POINT ( 'NONE',  ( 3.569546097624230807, 0.9179547258387925623, 0.3971843845618320268 ) ) ;
#15073 = CARTESIAN_POINT ( 'NONE',  ( 4.135359820172126000, 1.724334728327786559, 0.7510612840505229704 ) ) ;
#15074 = CARTESIAN_POINT ( 'NONE',  ( 2.124999999999999556, 0.000000000000000000, 2.500000000000000444 ) ) ;
#15075 = AXIS2_PLACEMENT_3D ( 'NONE', #115, #2590, #9408 ) ;
#15076 = CARTESIAN_POINT ( 'NONE',  ( 0.6179999999999965521, 1.679378605318035733, -2.054378605318066153 ) ) ;
#15077 = ORIENTED_EDGE ( 'NONE', *, *, #4474, .F. ) ;
#15078 = CARTESIAN_POINT ( 'NONE',  ( 0.6610344722576410037, 0.006457978392468126209, -0.4833528575413041928 ) ) ;
#15079 = EDGE_LOOP ( 'NONE', ( #11396, #11388, #426, #783 ) ) ;
#15080 = DIRECTION ( 'NONE',  ( 1.000000000000000000, 0.000000000000000000, 0.000000000000000000 ) ) ;
#15081 = CIRCLE ( 'NONE', #14339, 1.125000000000000888 ) ;
#15082 = CARTESIAN_POINT ( 'NONE',  ( 3.045371920833404467, 0.6267721954701572784, -0.3972696057387546387 ) ) ;
#15083 = DIRECTION ( 'NONE',  ( 0.000000000000000000, 0.000000000000000000, -1.000000000000000000 ) ) ;
#15084 = FACE_OUTER_BOUND ( 'NONE', #9601, .T. ) ;
#15085 = ORIENTED_EDGE ( 'NONE', *, *, #3996, .T. ) ;
#15086 = EDGE_CURVE ( 'NONE', #7643, #11264, #5972, .T. ) ;
#15087 = CARTESIAN_POINT ( 'NONE',  ( 0.7513246802501652999, -0.4429999999999999494, 0.4293820849162024444 ) ) ;
#15088 = ADVANCED_FACE ( 'NONE', ( #2383 ), #2299, .T. ) ;
#15089 = CARTESIAN_POINT ( 'NONE',  ( 0.7251620530230687978, -0.2214999999999999469, 0.5497635826929317959 ) ) ;
#15090 = ORIENTED_EDGE ( 'NONE', *, *, #13537, .T. ) ;
#15091 = FACE_OUTER_BOUND ( 'NONE', #2697, .T. ) ;
#15092 = VERTEX_POINT ( 'NONE', #5750 ) ;
#15093 = AXIS2_PLACEMENT_3D ( 'NONE', #11966, #1394, #10519 ) ;
#15094 = CARTESIAN_POINT ( 'NONE',  ( 2.774999999999999911, -1.679378605318059048, -1.679378605318041950 ) ) ;
#15095 = EDGE_LOOP ( 'NONE', ( #3619, #3686, #5724, #4699 ) ) ;
#15096 = CARTESIAN_POINT ( 'NONE',  ( 2.774999999999999911, 2.359999999999999876, -1.575000000000016831 ) ) ;
#15097 = CARTESIAN_POINT ( 'NONE',  ( 1.254789639631328058, -0.3704945895125943411, -0.4822769824910831393 ) ) ;
#15098 = DIRECTION ( 'NONE',  ( -0.7071067811865460184, 8.659560562354951347E-17, -0.7071067811865490160 ) ) ;
#15099 = B_SPLINE_CURVE_WITH_KNOTS ( 'NONE', 3,
 ( #9090, #7863, #11299, #11379, #12513, #648, #3043, #13583, #7712, #5572, #13733, #6646, #11231, #3127, #12370, #10091, #1884, #6574 ),
 .UNSPECIFIED., .F., .F.,
 ( 4, 2, 2, 2, 2, 2, 2, 2, 4 ),
 ( 4.557956953634194787E-07, 0.003683485157311049835, 0.005524999838118879909, 0.007366514518926710851, 0.008287271859330638465, 0.009208029199734566947, 0.01104954388054238575, 0.01289105856135020454, 0.01473257324215802161 ),
 .UNSPECIFIED. ) ;
#15100 = CIRCLE ( 'NONE', #12411, 0.1068000000000000754 ) ;
#15101 = CYLINDRICAL_SURFACE ( 'NONE', #5533, 0.2624999999999997335 ) ;
#15102 = CIRCLE ( 'NONE', #3385, 1.000000000000000000 ) ;
#15103 = VERTEX_POINT ( 'NONE', #3611 ) ;
#15104 = AXIS2_PLACEMENT_3D ( 'NONE', #6513, #14610, #5442 ) ;
#15105 = VERTEX_POINT ( 'NONE', #12934 ) ;
#15106 = AXIS2_PLACEMENT_3D ( 'NONE', #3366, #10327, #4595 ) ;
#15107 = FACE_BOUND ( 'NONE', #6378, .T. ) ;
#15108 = EDGE_LOOP ( 'NONE', ( #1255, #12179, #5578, #9151 ) ) ;
#15109 = CONICAL_SURFACE ( 'NONE', #8535, 0.2944999999999998175, 0.7853981633974520538 ) ;
#15110 = DIRECTION ( 'NONE',  ( -1.000000000000000000, -0.000000000000000000, -0.000000000000000000 ) ) ;
#15111 = LINE ( 'NONE', #7172, #5919 ) ;
#15113 = DIRECTION ( 'NONE',  ( -0.000000000000000000, -1.000000000000000000, -0.000000000000000000 ) ) ;
#15112 = CIRCLE ( 'NONE', #2171, 0.2625000000000000111 ) ;
#15114 = CARTESIAN_POINT ( 'NONE',  ( 0.7176122613104025660, -0.008225492514568092176, -0.4611624156322176038 ) ) ;
#15115 = EDGE_LOOP ( 'NONE', ( #12456, #9076 ) ) ;
#15116 = FACE_OUTER_BOUND ( 'NONE', #2243, .T. ) ;
#15117 = CARTESIAN_POINT ( 'NONE',  ( 0.6552615383573133778, -0.03272338206886943324, -0.5074994761915084807 ) ) ;
#15118 = DIRECTION ( 'NONE',  ( -0.7071067811865350272, 0.7071067811865600072, 0.000000000000000000 ) ) ;
#15119 = AXIS2_PLACEMENT_3D ( 'NONE', #1745, #7728, #11166 ) ;
#15120 = EDGE_CURVE ( 'NONE', #626, #4833, #5646, .T. ) ;
#15121 = EDGE_CURVE ( 'NONE', #5634, #9649, #3692, .T. ) ;
#15122 = EDGE_CURVE ( 'NONE', #2273, #12566, #7432, .T. ) ;
#15123=STYLED_ITEM('',(#15171),#10641);
#15124 = VECTOR ( 'NONE', #8550, 39.37007874015748143 ) ;
#15125 =( LENGTH_UNIT ( ) NAMED_UNIT ( * ) SI_UNIT ( $, .METRE. ) );
#15126 = CARTESIAN_POINT ( 'NONE',  ( 4.663405195611884047, 1.729552445905039981, -0.1874371909834770533 ) ) ;
#15127 = VERTEX_POINT ( 'NONE', #11489 ) ;
#15129 = VERTEX_POINT ( 'NONE', #6981 ) ;
#15128 = DIRECTION ( 'NONE',  ( 0.000000000000000000, 0.000000000000000000, 1.000000000000000000 ) ) ;
#15130 = EDGE_CURVE ( 'NONE', #4870, #6979, #4525, .T. ) ;
#15131 = ORIENTED_EDGE ( 'NONE', *, *, #9058, .T. ) ;
#15133 = ORIENTED_EDGE ( 'NONE', *, *, #11291, .T. ) ;
#15132 = DIRECTION ( 'NONE',  ( 0.000000000000000000, 0.000000000000000000, -1.000000000000000000 ) ) ;
#15134 = ORIENTED_EDGE ( 'NONE', *, *, #14739, .F. ) ;
#15135 = DIRECTION ( 'NONE',  ( -0.000000000000000000, -1.000000000000000000, -0.000000000000000000 ) ) ;
#15136 = LENGTH_MEASURE_WITH_UNIT ( LENGTH_MEASURE( 0.02539999999999999897 ), #2978 );
#15137 = FACE_BOUND ( 'NONE', #9249, .T. ) ;
#15138 = EDGE_LOOP ( 'NONE', ( #3674, #11215, #3993, #12264 ) ) ;
#15139 = CIRCLE ( 'NONE', #8552, 0.3440000000000000280 ) ;
#15140 = FACE_OUTER_BOUND ( 'NONE', #9387, .T. ) ;
#15141 = DIRECTION ( 'NONE',  ( -1.224646799147352961E-16, 0.000000000000000000, -1.000000000000000000 ) ) ;
#15142 = VECTOR ( 'NONE', #5381, 39.37007874015748143 ) ;
#15143 = CARTESIAN_POINT ( 'NONE',  ( 0.000000000000000000, 0.000000000000000000, 0.000000000000000000 ) ) ;
#15144 = DIRECTION ( 'NONE',  ( -1.000000000000000000, -0.000000000000000000, -0.000000000000000000 ) ) ;
#15145 = DIRECTION ( 'NONE',  ( 0.000000000000000000, 0.000000000000000000, -1.000000000000000000 ) ) ;
#15146 = CARTESIAN_POINT ( 'NONE',  ( 2.124999999999999556, 0.000000000000000000, 0.000000000000000000 ) ) ;
#15147 = FACE_OUTER_BOUND ( 'NONE', #12133, .T. ) ;
#15148 = CARTESIAN_POINT ( 'NONE',  ( 3.426491571325181340, 1.679378605318059048, 1.416878605318041551 ) ) ;
#15149 = FACE_OUTER_BOUND ( 'NONE', #2768, .T. ) ;
#15150 = CIRCLE ( 'NONE', #467, 0.9499999999999988454 ) ;
#15151 = VERTEX_POINT ( 'NONE', #10419 ) ;
#15152 = CARTESIAN_POINT ( 'NONE',  ( -0.7287617923574205570, 0.2159999999999999420, 0.4425000000000005596 ) ) ;
#15153 = NEXT_ASSEMBLY_USAGE_OCCURRENCE ( 'NAUO1', ' ', ' ', #4715, #14914, $ ) ;
#15154 = NEXT_ASSEMBLY_USAGE_OCCURRENCE ( 'NAUO2', ' ', ' ', #4715, #13772, $ ) ;
#15155 = NEXT_ASSEMBLY_USAGE_OCCURRENCE ( 'NAUO3', ' ', ' ', #4715, #1525, $ ) ;
#15156 = NEXT_ASSEMBLY_USAGE_OCCURRENCE ( 'NAUO4', ' ', ' ', #4715, #1525, $ ) ;
#15157 = NEXT_ASSEMBLY_USAGE_OCCURRENCE ( 'NAUO5', ' ', ' ', #4715, #1525, $ ) ;
#15158 = NEXT_ASSEMBLY_USAGE_OCCURRENCE ( 'NAUO6', ' ', ' ', #4715, #1525, $ ) ;
#15159 = NEXT_ASSEMBLY_USAGE_OCCURRENCE ( 'NAUO7', ' ', ' ', #4715, #3599, $ ) ;
#15160 = NEXT_ASSEMBLY_USAGE_OCCURRENCE ( 'NAUO8', ' ', ' ', #4715, #869, $ ) ;
#15161 = NEXT_ASSEMBLY_USAGE_OCCURRENCE ( 'NAUO9', ' ', ' ', #4715, #3615, $ ) ;
#15162 = NEXT_ASSEMBLY_USAGE_OCCURRENCE ( 'NAUO10', ' ', ' ', #4715, #6322, $ ) ;
#15163 = NEXT_ASSEMBLY_USAGE_OCCURRENCE ( 'NAUO11', ' ', ' ', #4715, #2485, $ ) ;
#15164 = NEXT_ASSEMBLY_USAGE_OCCURRENCE ( 'NAUO12', ' ', ' ', #4715, #2485, $ ) ;
#15165=COLOUR_RGB('Dark Blue',0.08,0.2,0.34);
#15166=FILL_AREA_STYLE_COLOUR('',#15165);
#15167=FILL_AREA_STYLE('',(#15166));
#15168=SURFACE_STYLE_FILL_AREA(#15167);
#15169=SURFACE_SIDE_STYLE('',(#15168));
#15170=SURFACE_STYLE_USAGE(.BOTH.,#15169);
#15171=PRESENTATION_STYLE_ASSIGNMENT((#15170));
#15172=COLOUR_RGB('Light Blue',0.38,0.62,0.78);
#15173=FILL_AREA_STYLE_COLOUR('',#15172);
#15174=FILL_AREA_STYLE('',(#15173));
#15175=SURFACE_STYLE_FILL_AREA(#15174);
#15176=SURFACE_SIDE_STYLE('',(#15175));
#15177=SURFACE_STYLE_USAGE(.BOTH.,#15176);
#15178=PRESENTATION_STYLE_ASSIGNMENT((#15177));
#15179=COLOUR_RGB('Sky Blue',0.24,0.69,0.87);
#15180=FILL_AREA_STYLE_COLOUR('',#15179);
#15181=FILL_AREA_STYLE('',(#15180));
#15182=SURFACE_STYLE_FILL_AREA(#15181);
#15183=SURFACE_SIDE_STYLE('',(#15182));
#15184=SURFACE_STYLE_USAGE(.BOTH.,#15183);
#15185=PRESENTATION_STYLE_ASSIGNMENT((#15184));
#15186=COLOUR_RGB('Grey',0.48,0.52,0.57);
#15187=FILL_AREA_STYLE_COLOUR('',#15186);
#15188=FILL_AREA_STYLE('',(#15187));
#15189=SURFACE_STYLE_FILL_AREA(#15188);
#15190=SURFACE_SIDE_STYLE('',(#15189));
#15191=SURFACE_STYLE_USAGE(.BOTH.,#15190);
#15192=PRESENTATION_STYLE_ASSIGNMENT((#15191));
#15193=COLOUR_RGB('Black',0.12,0.14,0.17);
#15194=FILL_AREA_STYLE_COLOUR('',#15193);
#15195=FILL_AREA_STYLE('',(#15194));
#15196=SURFACE_STYLE_FILL_AREA(#15195);
#15197=SURFACE_SIDE_STYLE('',(#15196));
#15198=SURFACE_STYLE_USAGE(.BOTH.,#15197);
#15199=PRESENTATION_STYLE_ASSIGNMENT((#15198));
#15200=COLOUR_RGB('Off White',0.89,0.88,0.83);
#15201=FILL_AREA_STYLE_COLOUR('',#15200);
#15202=FILL_AREA_STYLE('',(#15201));
#15203=SURFACE_STYLE_FILL_AREA(#15202);
#15204=SURFACE_SIDE_STYLE('',(#15203));
#15205=SURFACE_STYLE_USAGE(.BOTH.,#15204);
#15206=PRESENTATION_STYLE_ASSIGNMENT((#15205));
ENDSEC;
END-ISO-10303-21;
